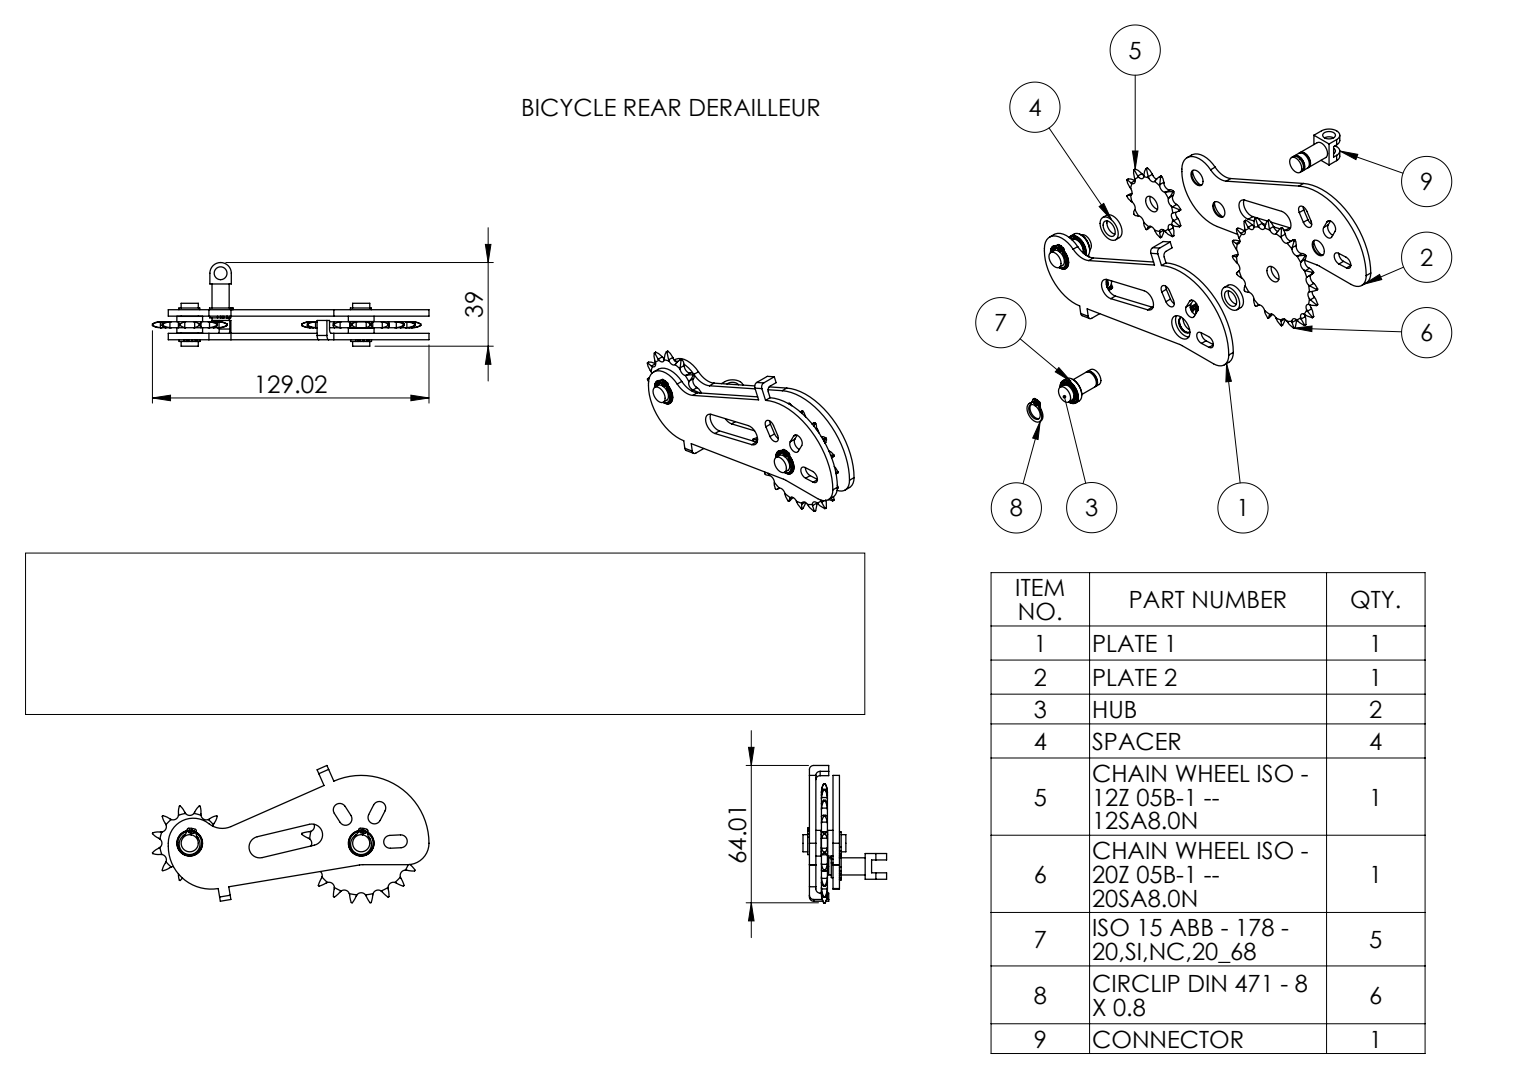
ISO-10303-21;
HEADER;
FILE_DESCRIPTION (('STEP AP214'),
    '1' );
FILE_NAME ('MAS-167',
    '2026-10-31T03:41:51',
    ( '' ),
    ( '' ),
    'SwSTEP 2.0',
    'SolidWorks 2026',
    '' );
FILE_SCHEMA (( 'AUTOMOTIVE_DESIGN' ));
ENDSEC;

DATA;
#1 = DIRECTION ( 'NONE',  ( 0.000000000000000000, 0.000000000000000000, 1.000000000000000000 ) ) ;
#2 = CARTESIAN_POINT ( 'NONE',  ( 1.749999999999998002, 19.67366047555530528, 20.02152543075352753 ) ) ;
#3 = CARTESIAN_POINT ( 'NONE',  ( 0.000000000000000000, 0.000000000000000000, 0.000000000000000000 ) ) ;
#4 = ORIENTED_EDGE ( 'NONE', *, *, #1307, .T. ) ;
#5 = CARTESIAN_POINT ( 'NONE',  ( 67.45386469005195806, 13.93318132202354676, 7.000000000000000000 ) ) ;
#6 = EDGE_LOOP ( 'NONE', ( #14602, #6535, #10108, #15176, #740, #8650, #3309 ) ) ;
#7 = DIRECTION ( 'NONE',  ( -1.000000000000000000, -0.000000000000000000, -0.000000000000000000 ) ) ;
#8 = CARTESIAN_POINT ( 'NONE',  ( 1.749999999999999778, 0.000000000000000000, 0.000000000000000000 ) ) ;
#9 = ORIENTED_EDGE ( 'NONE', *, *, #4269, .F. ) ;
#10 = ORIENTED_EDGE ( 'NONE', *, *, #14463, .T. ) ;
#11 = EDGE_CURVE ( 'NONE', #14793, #10954, #11402, .T. ) ;
#12 = CARTESIAN_POINT ( 'NONE',  ( 0.000000000000000000, 0.000000000000000000, 5.000000000000000000 ) ) ;
#13 = ORIENTED_EDGE ( 'NONE', *, *, #14923, .F. ) ;
#14 = DIRECTION ( 'NONE',  ( -0.9873505073845697533, 0.1585527532634883052, 0.000000000000000000 ) ) ;
#15 = CARTESIAN_POINT ( 'NONE',  ( 3.510166481118872639, 1.455586230640303791, -7.000000000000007994 ) ) ;
#16 = CARTESIAN_POINT ( 'NONE',  ( 0.7592463834391185440, 12.05220173035438513, 24.80264696524887214 ) ) ;
#17 = DIRECTION ( 'NONE',  ( 1.000000000000000000, 0.000000000000000000, 0.000000000000000000 ) ) ;
#18 = ORIENTED_EDGE ( 'NONE', *, *, #2231, .T. ) ;
#19 = FACE_OUTER_BOUND ( 'NONE', #11949, .T. ) ;
#20 = CARTESIAN_POINT ( 'NONE',  ( 0.02531912748631424959, 14.46287784598617243, 2.311161484776605324 ) ) ;
#21 = ORIENTED_EDGE ( 'NONE', *, *, #15147, .T. ) ;
#22 = ORIENTED_EDGE ( 'NONE', *, *, #685, .T. ) ;
#23 = CARTESIAN_POINT ( 'NONE',  ( 2.718184745196084773, 21.92234060054363809, -12.74223776959176568 ) ) ;
#24 = CARTESIAN_POINT ( 'NONE',  ( 0.006931054464085539824, -24.42321038836781355, -2.248820353273226491 ) ) ;
#25 = LINE ( 'NONE', #3651, #6082 ) ;
#26 = CARTESIAN_POINT ( 'NONE',  ( 101.4858053992934401, 0.9022481406819604643, 7.000000000000000000 ) ) ;
#27 = DIRECTION ( 'NONE',  ( 1.000000000000000000, 0.000000000000000000, 0.000000000000000000 ) ) ;
#28 = DIRECTION ( 'NONE',  ( -1.000000000000000000, 0.000000000000000000, 0.000000000000000000 ) ) ;
#29 = EDGE_CURVE ( 'NONE', #14731, #12050, #4275, .T. ) ;
#30 = ORIENTED_EDGE ( 'NONE', *, *, #9953, .F. ) ;
#31 = FACE_BOUND ( 'NONE', #5073, .T. ) ;
#32 = CARTESIAN_POINT ( 'NONE',  ( 1.039999999999997593, 0.000000000000000000, 0.000000000000000000 ) ) ;
#33 = CARTESIAN_POINT ( 'NONE',  ( 0.02531912748606228100, 5.229914364928351489, 13.68080036884350292 ) ) ;
#34 = DIRECTION ( 'NONE',  ( -1.000000000000000000, 0.000000000000000000, -0.000000000000000000 ) ) ;
#35 = VECTOR ( 'NONE', #190, 1000.000000000000000 ) ;
#36 = ORIENTED_EDGE ( 'NONE', *, *, #1393, .T. ) ;
#37 = EDGE_CURVE ( 'NONE', #40, #2037, #3752, .T. ) ;
#38 = EDGE_LOOP ( 'NONE', ( #950, #5937 ) ) ;
#39 = CARTESIAN_POINT ( 'NONE',  ( 0.07186813532171011654, 25.22589920183360945, 2.577209017047096484 ) ) ;
#40 = VERTEX_POINT ( 'NONE', #3206 ) ;
#41 = CARTESIAN_POINT ( 'NONE',  ( 2.597943782557557313, 12.05486625177586113, -10.28947301956269733 ) ) ;
#42 = CYLINDRICAL_SURFACE ( 'NONE', #425, 5.999999999999999112 ) ;
#43 = DIRECTION ( 'NONE',  ( -0.9863939238321437486, -0.1643989873053572359, 0.000000000000000000 ) ) ;
#44 = CARTESIAN_POINT ( 'NONE',  ( 67.45386469005195806, 13.93318132202354676, 4.000000000000000000 ) ) ;
#45 = FACE_OUTER_BOUND ( 'NONE', #11478, .T. ) ;
#46 = EDGE_CURVE ( 'NONE', #11802, #6223, #12333, .T. ) ;
#47 = EDGE_CURVE ( 'NONE', #3966, #1296, #12443, .T. ) ;
#48 = DIRECTION ( 'NONE',  ( 1.000000000000000000, 0.000000000000000000, 0.000000000000000000 ) ) ;
#49 = CARTESIAN_POINT ( 'NONE',  ( -14.40394475573011945, -10.79473832354794460, -3.794707603699265519E-15 ) ) ;
#50 = ORIENTED_EDGE ( 'NONE', *, *, #12668, .F. ) ;
#51 = CARTESIAN_POINT ( 'NONE',  ( 69.97572749000833880, 15.55805301486455683, 6.000000000000000000 ) ) ;
#52 = ORIENTED_EDGE ( 'NONE', *, *, #8148, .F. ) ;
#53 = B_SPLINE_CURVE_WITH_KNOTS ( 'NONE', 3,
 ( #7309, #10834, #290, #4708, #9377, #14064, #7077, #10905 ),
 .UNSPECIFIED., .F., .F.,
 ( 4, 2, 2, 4 ),
 ( 1.984117563342701228E-07, 0.001895214258086351869, 0.002842722181251365696, 0.003790230104416379524 ),
 .UNSPECIFIED. ) ;
#54 = ORIENTED_EDGE ( 'NONE', *, *, #8757, .F. ) ;
#55 = EDGE_LOOP ( 'NONE', ( #13749, #2858, #11395, #485, #2000, #143, #1377, #4123 ) ) ;
#56 = ORIENTED_EDGE ( 'NONE', *, *, #14923, .T. ) ;
#57 = DIRECTION ( 'NONE',  ( 0.9863939238321437486, 0.1643989873053572359, -0.000000000000000000 ) ) ;
#58 = EDGE_CURVE ( 'NONE', #2051, #1778, #6057, .T. ) ;
#59 = CARTESIAN_POINT ( 'NONE',  ( 2.257825459230520693, -26.58873630738055738, 4.993157874727710777 ) ) ;
#60 = CARTESIAN_POINT ( 'NONE',  ( 0.02436607992776151574, -16.37294372382871188, 18.55949924794887096 ) ) ;
#61 = DIRECTION ( 'NONE',  ( 1.000000000000000000, -0.000000000000000000, 0.000000000000000000 ) ) ;
#62 = EDGE_CURVE ( 'NONE', #4667, #5041, #11487, .T. ) ;
#63 = CARTESIAN_POINT ( 'NONE',  ( 2.021362784118872380, 12.71987259277435101, 11.98841295390602291 ) ) ;
#64 = ORIENTED_EDGE ( 'NONE', *, *, #823, .T. ) ;
#65 = DIRECTION ( 'NONE',  ( 1.000000000000000000, 0.000000000000000000, 0.000000000000000000 ) ) ;
#66 = ADVANCED_FACE ( 'NONE', ( #13569 ), #14807, .T. ) ;
#67 = PRODUCT_DEFINITION_FORMATION_WITH_SPECIFIED_SOURCE ( 'ANY', '', #14008, .NOT_KNOWN. ) ;
#68 = B_SPLINE_CURVE_WITH_KNOTS ( 'NONE', 3,
 ( #9226, #12751, #12598, #7922 ),
 .UNSPECIFIED., .F., .F.,
 ( 4, 4 ),
 ( 0.005258214619651953650, 0.005948481662034169060 ),
 .UNSPECIFIED. ) ;
#69 = ORIENTED_EDGE ( 'NONE', *, *, #13888, .F. ) ;
#70 = DIRECTION ( 'NONE',  ( -1.000000000000000000, 0.000000000000000000, -0.000000000000000000 ) ) ;
#71 = CARTESIAN_POINT ( 'NONE',  ( 2.321707774797442170, -4.824281976789052351, -0.8000000000000000444 ) ) ;
#72 = ORIENTED_EDGE ( 'NONE', *, *, #10132, .F. ) ;
#73 = ORIENTED_EDGE ( 'NONE', *, *, #10146, .F. ) ;
#74 = VECTOR ( 'NONE', #9395, 1000.000000000000000 ) ;
#75 = CARTESIAN_POINT ( 'NONE',  ( 1.039999999999996705, -20.02152543075359503, 19.67366047555523423 ) ) ;
#76 = ORIENTED_EDGE ( 'NONE', *, *, #9574, .F. ) ;
#77 = CARTESIAN_POINT ( 'NONE',  ( 1.394999999999998685, -17.29145405592685592, -4.835383649608655077 ) ) ;
#78 = DIRECTION ( 'NONE',  ( 0.000000000000000000, 0.000000000000000000, 1.000000000000000000 ) ) ;
#79 = CIRCLE ( 'NONE', #12614, 2.524999999999995914 ) ;
#80 = EDGE_CURVE ( 'NONE', #14477, #12497, #893, .T. ) ;
#81 = LINE ( 'NONE', #4807, #9670 ) ;
#82 = DIRECTION ( 'NONE',  ( 1.000000000000000000, 0.000000000000000000, 0.000000000000000000 ) ) ;
#83 = AXIS2_PLACEMENT_3D ( 'NONE', #12393, #1953, #3185 ) ;
#84 = TOROIDAL_SURFACE ( 'NONE', #8934, 5.000000000000000000, 0.5999999999999999778 ) ;
#85 = VERTEX_POINT ( 'NONE', #12565 ) ;
#86 = DIRECTION ( 'NONE',  ( -1.000000000000000000, -0.000000000000000000, 0.000000000000000000 ) ) ;
#87 = DIRECTION ( 'NONE',  ( -1.000000000000000000, 0.000000000000000000, -0.000000000000000000 ) ) ;
#88 = ORIENTED_EDGE ( 'NONE', *, *, #2042, .F. ) ;
#89 = ORIENTED_EDGE ( 'NONE', *, *, #1488, .F. ) ;
#90 = CARTESIAN_POINT ( 'NONE',  ( 0.07473575470096445461, -11.74839219818081482, -9.749517823374134196 ) ) ;
#92 = CARTESIAN_POINT ( 'NONE',  ( 0.000000000000000000, 24.34211360614310848, -7.909232158574561744 ) ) ;
#91 = AXIS2_PLACEMENT_3D ( 'NONE', #9821, #7739, #5069 ) ;
#93 = AXIS2_PLACEMENT_3D ( 'NONE', #1649, #1959, #6645 ) ;
#94 = LINE ( 'NONE', #4592, #6321 ) ;
#95 = CARTESIAN_POINT ( 'NONE',  ( -14.40394475573011945, -2.082238426203170629E-15, 16.99999999999999645 ) ) ;
#96 = DIRECTION ( 'NONE',  ( -1.000000000000000000, 0.000000000000000000, 0.000000000000000000 ) ) ;
#97 = ADVANCED_FACE ( 'NONE', ( #2039 ), #6726, .F. ) ;
#98 = DIRECTION ( 'NONE',  ( 0.000000000000000000, 0.000000000000000000, -1.000000000000000000 ) ) ;
#99 = VERTEX_POINT ( 'NONE', #962 ) ;
#100 = CARTESIAN_POINT ( 'NONE',  ( 72.68384697807672978, 11.35494834827056110, 7.000000000000000000 ) ) ;
#101 = DIRECTION ( 'NONE',  ( 0.000000000000000000, 0.000000000000000000, 1.000000000000000000 ) ) ;
#102 = DIRECTION ( 'NONE',  ( 0.9021244663126475327, 0.4314758942051350465, -1.141265444721583757E-16 ) ) ;
#103 = LINE ( 'NONE', #14195, #2432 ) ;
#104 = AXIS2_PLACEMENT_3D ( 'NONE', #9255, #12995, #7014 ) ;
#105 = DIRECTION ( 'NONE',  ( 1.000000000000000000, 0.000000000000000000, 0.000000000000000000 ) ) ;
#106 = ORIENTED_EDGE ( 'NONE', *, *, #6088, .F. ) ;
#107 = VECTOR ( 'NONE', #15180, 1000.000000000000114 ) ;
#108 = VERTEX_POINT ( 'NONE', #10337 ) ;
#109 = EDGE_CURVE ( 'NONE', #389, #2825, #14096, .T. ) ;
#110 = ORIENTED_EDGE ( 'NONE', *, *, #7513, .T. ) ;
#111 = CARTESIAN_POINT ( 'NONE',  ( 1.749999999999999778, 17.39253030560841395, -4.458161950358560333 ) ) ;
#112 = CYLINDRICAL_SURFACE ( 'NONE', #13936, 11.66666666666667318 ) ;
#113 = EDGE_CURVE ( 'NONE', #13456, #5828, #10676, .T. ) ;
#114 = CARTESIAN_POINT ( 'NONE',  ( 0.5537796329733287726, 5.139875429511856275, 16.15122426806991385 ) ) ;
#115 = CARTESIAN_POINT ( 'NONE',  ( 2.740003299868483566, 9.490919315500294218, -11.55877992729655368 ) ) ;
#116 = CARTESIAN_POINT ( 'NONE',  ( 0.000000000000000000, 0.000000000000000000, -7.000000000000008882 ) ) ;
#117 = CARTESIAN_POINT ( 'NONE',  ( 76.00000000000000000, 4.898587196589422689E-16, 6.000000000000000000 ) ) ;
#118 = CIRCLE ( 'NONE', #10455, 4.999999999999997335 ) ;
#119 = CIRCLE ( 'NONE', #7473, 14.01039946648074341 ) ;
#120 = ORIENTED_EDGE ( 'NONE', *, *, #11422, .T. ) ;
#121 = DIRECTION ( 'NONE',  ( 0.000000000000000000, 0.000000000000000000, 1.000000000000000000 ) ) ;
#122 = CARTESIAN_POINT ( 'NONE',  ( 50.00050000000000239, 0.000000000000000000, 4.000000000000000000 ) ) ;
#123 = EDGE_LOOP ( 'NONE', ( #11142, #6694, #3229, #3331, #1477 ) ) ;
#124 = DIRECTION ( 'NONE',  ( -1.000000000000000000, -0.000000000000000000, -0.000000000000000000 ) ) ;
#125 = PLANE ( 'NONE',  #1631 ) ;
#126 = PRODUCT_DEFINITION_SHAPE ( 'NONE', 'NONE',  #15227 ) ;
#127 = FILL_AREA_STYLE_COLOUR ( '', #7232 ) ;
#128 = EDGE_LOOP ( 'NONE', ( #4298, #9010, #776, #2710 ) ) ;
#129 = CIRCLE ( 'NONE', #8981, 24.12539914357697768 ) ;
#130 = EDGE_CURVE ( 'NONE', #2515, #5688, #11223, .T. ) ;
#131 = PRESENTATION_STYLE_ASSIGNMENT (( #7148 ) ) ;
#132 = VERTEX_POINT ( 'NONE', #20 ) ;
#133 = EDGE_LOOP ( 'NONE', ( #203, #10433, #5275, #14056, #9292, #1957 ) ) ;
#134 = VERTEX_POINT ( 'NONE', #3643 ) ;
#135 = CARTESIAN_POINT ( 'NONE',  ( 80.00000000000000000, 0.000000000000000000, 5.500000000000000000 ) ) ;
#136 = FACE_BOUND ( 'NONE', #13544, .T. ) ;
#137 = CARTESIAN_POINT ( 'NONE',  ( 101.6227766016837819, 5.204170427930421283E-15, -130.1575142076926852 ) ) ;
#138 = DIRECTION ( 'NONE',  ( -0.000000000000000000, -0.000000000000000000, 1.000000000000000000 ) ) ;
#139 = CIRCLE ( 'NONE', #11189, 3.799999999999999378 ) ;
#140 = EDGE_CURVE ( 'NONE', #12264, #4663, #14022, .T. ) ;
#141 = CARTESIAN_POINT ( 'NONE',  ( 0.7589665349472735079, 4.828387785248019703, 27.14933624560909919 ) ) ;
#142 = AXIS2_PLACEMENT_3D ( 'NONE', #6608, #14906, #1917 ) ;
#143 = ORIENTED_EDGE ( 'NONE', *, *, #12762, .T. ) ;
#144 = CARTESIAN_POINT ( 'NONE',  ( 0.000000000000000000, 0.000000000000000000, 3.895000000000000462 ) ) ;
#145 = VECTOR ( 'NONE', #5198, 1000.000000000000000 ) ;
#146 = EDGE_CURVE ( 'NONE', #14971, #5007, #13767, .T. ) ;
#147 = ADVANCED_FACE ( 'NONE', ( #4891 ), #11848, .T. ) ;
#148 = CIRCLE ( 'NONE', #8022, 2.524999999999995914 ) ;
#149 =( REPRESENTATION_RELATIONSHIP ('NONE','NONE', #12685, #2588 ) REPRESENTATION_RELATIONSHIP_WITH_TRANSFORMATION ( #14747 )SHAPE_REPRESENTATION_RELATIONSHIP( ) );
#150 = EDGE_LOOP ( 'NONE', ( #5698, #6923, #12784, #4888 ) ) ;
#151 = DIRECTION ( 'NONE',  ( -0.8406209333187997235, -0.5416238976136763528, 0.000000000000000000 ) ) ;
#152 = CARTESIAN_POINT ( 'NONE',  ( 1.039999999999996261, -17.29145405592685592, -4.835383649608655077 ) ) ;
#153 = EDGE_LOOP ( 'NONE', ( #4267, #3860, #12401, #12111, #6299, #3424, #1299, #11169 ) ) ;
#154 = VERTEX_POINT ( 'NONE', #3488 ) ;
#155 = AXIS2_PLACEMENT_3D ( 'NONE', #13835, #4322, #4404 ) ;
#156 = CIRCLE ( 'NONE', #8761, 0.7500000000000002220 ) ;
#157 = VECTOR ( 'NONE', #9903, 1000.000000000000000 ) ;
#158 = DIRECTION ( 'NONE',  ( 1.000000000000000000, 0.000000000000000000, 0.000000000000000000 ) ) ;
#159 = VERTEX_POINT ( 'NONE', #10494 ) ;
#160 = VECTOR ( 'NONE', #9182, 1000.000000000000000 ) ;
#161 = LINE ( 'NONE', #4805, #11382 ) ;
#162 = CARTESIAN_POINT ( 'NONE',  ( -16.14082873121598993, -7.414910804916202913, -3.000000000000000000 ) ) ;
#163 = EDGE_CURVE ( 'NONE', #12063, #1974, #3422, .T. ) ;
#164 = ADVANCED_FACE ( 'NONE', ( #8330 ), #7536, .T. ) ;
#165 = DIRECTION ( 'NONE',  ( 0.000000000000000000, 0.8660254037844327124, 0.5000000000000104361 ) ) ;
#166 = FACE_OUTER_BOUND ( 'NONE', #10902, .T. ) ;
#167 = AXIS2_PLACEMENT_3D ( 'NONE', #499, #13191, #7439 ) ;
#168 = EDGE_LOOP ( 'NONE', ( #13851, #5539, #1139, #30 ) ) ;
#169 = DIRECTION ( 'NONE',  ( -0.9148936170212769170, -0.4036950204470262649, 0.000000000000000000 ) ) ;
#170 = EDGE_CURVE ( 'NONE', #1510, #11203, #8177, .T. ) ;
#171 = CARTESIAN_POINT ( 'NONE',  ( 1.039999999999997371, 4.458161950358744186, -17.39253030560836777 ) ) ;
#172 = AXIS2_PLACEMENT_3D ( 'NONE', #5466, #3375, #833 ) ;
#173 = CIRCLE ( 'NONE', #4631, 14.01039946648074341 ) ;
#174 = ORIENTED_EDGE ( 'NONE', *, *, #12406, .F. ) ;
#175 = DIRECTION ( 'NONE',  ( 1.000000000000000000, 0.000000000000000000, 0.000000000000000000 ) ) ;
#176 = EDGE_LOOP ( 'NONE', ( #1544, #7262 ) ) ;
#177 = ORIENTED_EDGE ( 'NONE', *, *, #10181, .F. ) ;
#178 = DIRECTION ( 'NONE',  ( 0.9148936170212770280, 0.4036950204470263204, -0.000000000000000000 ) ) ;
#179 = DIRECTION ( 'NONE',  ( -0.9728364810787193395, -0.2314933715733012709, -0.000000000000000000 ) ) ;
#180 = EDGE_CURVE ( 'NONE', #10751, #7956, #7783, .T. ) ;
#181 = AXIS2_PLACEMENT_3D ( 'NONE', #7000, #4114, #12760 ) ;
#182 = CARTESIAN_POINT ( 'NONE',  ( 2.782672467460656218, 14.24942254254689189, 2.217238903388611071 ) ) ;
#183 = CARTESIAN_POINT ( 'NONE',  ( -10.00000000000000000, 0.000000000000000000, 0.000000000000000000 ) ) ;
#184 = DIRECTION ( 'NONE',  ( -1.000000000000000000, -0.000000000000000000, -0.000000000000000000 ) ) ;
#185 = AXIS2_PLACEMENT_3D ( 'NONE', #6437, #12199, #1683 ) ;
#186 = PLANE ( 'NONE',  #13689 ) ;
#187 = AXIS2_PLACEMENT_3D ( 'NONE', #8087, #3532, #12761 ) ;
#188 = VERTEX_POINT ( 'NONE', #5888 ) ;
#189 = DIRECTION ( 'NONE',  ( -1.576560579138138762E-17, 1.359337748750801608E-17, -1.000000000000000000 ) ) ;
#190 = DIRECTION ( 'NONE',  ( 1.000000000000000000, -0.000000000000000000, -0.000000000000000000 ) ) ;
#191 = DIRECTION ( 'NONE',  ( -1.000000000000000000, 0.000000000000000000, 0.000000000000000000 ) ) ;
#192 = CARTESIAN_POINT ( 'NONE',  ( 2.789999999999999147, 22.25075486061738772, 9.324097380959527115 ) ) ;
#193 = ORIENTED_EDGE ( 'NONE', *, *, #9161, .T. ) ;
#194 = ORIENTED_EDGE ( 'NONE', *, *, #4990, .T. ) ;
#195 = ORIENTED_EDGE ( 'NONE', *, *, #10486, .F. ) ;
#196 = AXIS2_PLACEMENT_3D ( 'NONE', #5704, #8149, #10157 ) ;
#197 = CARTESIAN_POINT ( 'NONE',  ( 0.02436607992775674525, 9.836394144776026138, -22.71065055754441531 ) ) ;
#198 = CARTESIAN_POINT ( 'NONE',  ( 2.789999999999999147, 1.991882183130632589, -24.04302995059963877 ) ) ;
#199 = CARTESIAN_POINT ( 'NONE',  ( 0.07473581742173406040, 5.299647274067100788, 14.31752701692938778 ) ) ;
#200 = CARTESIAN_POINT ( 'NONE',  ( 2.246812931352481613, 11.42270873787310315, -12.54666350726111901 ) ) ;
#201 = DIRECTION ( 'NONE',  ( 1.000000000000000000, 0.000000000000000000, 0.000000000000000000 ) ) ;
#202 = DIRECTION ( 'NONE',  ( -0.000000000000000000, -0.000000000000000000, -1.000000000000000000 ) ) ;
#203 = ORIENTED_EDGE ( 'NONE', *, *, #12220, .F. ) ;
#204 = FACE_OUTER_BOUND ( 'NONE', #6, .T. ) ;
#205 = DIRECTION ( 'NONE',  ( 0.000000000000000000, 0.000000000000000000, 1.000000000000000000 ) ) ;
#206 = ORIENTED_EDGE ( 'NONE', *, *, #5456, .T. ) ;
#207 = DIRECTION ( 'NONE',  ( -1.000000000000000000, -0.000000000000000000, 0.000000000000000000 ) ) ;
#208 = CARTESIAN_POINT ( 'NONE',  ( 0.07473575470096512074, 9.749517823374169723, -11.74839219818077929 ) ) ;
#209 = VECTOR ( 'NONE', #6552, 1000.000000000000114 ) ;
#210 = FACE_OUTER_BOUND ( 'NONE', #11250, .T. ) ;
#211 = EDGE_CURVE ( 'NONE', #12769, #12700, #14657, .T. ) ;
#212 = VERTEX_POINT ( 'NONE', #10569 ) ;
#213 = ORIENTED_EDGE ( 'NONE', *, *, #12762, .F. ) ;
#214 = VERTEX_POINT ( 'NONE', #2422 ) ;
#215 = ORIENTED_EDGE ( 'NONE', *, *, #3281, .T. ) ;
#216 = CARTESIAN_POINT ( 'NONE',  ( 80.00000000000000000, 0.000000000000000000, -131.1575142076926852 ) ) ;
#217 = LINE ( 'NONE', #14226, #7341 ) ;
#218 = CARTESIAN_POINT ( 'NONE',  ( 2.790000000000009805, 5.211150952915548196, -13.21889893246969905 ) ) ;
#219 = DIRECTION ( 'NONE',  ( -1.000000000000000000, -0.000000000000000000, -0.000000000000000000 ) ) ;
#220 = CIRCLE ( 'NONE', #8093, 5.999999999999999112 ) ;
#221 = LINE ( 'NONE', #525, #10167 ) ;
#222 = DIRECTION ( 'NONE',  ( -1.000000000000000000, -0.000000000000000000, -0.000000000000000000 ) ) ;
#223 = ORIENTED_EDGE ( 'NONE', *, *, #14809, .T. ) ;
#224 = DIRECTION ( 'NONE',  ( -0.000000000000000000, -0.000000000000000000, -1.000000000000000000 ) ) ;
#225 = ADVANCED_FACE ( 'NONE', ( #6882 ), #11561, .F. ) ;
#226 = CIRCLE ( 'NONE', #8834, 6.000000000000005329 ) ;
#227 = EDGE_CURVE ( 'NONE', #9499, #4705, #4811, .T. ) ;
#228 = VERTEX_POINT ( 'NONE', #7180 ) ;
#229 = CYLINDRICAL_SURFACE ( 'NONE', #11421, 13.19999999999999929 ) ;
#230 = DIRECTION ( 'NONE',  ( 0.000000000000000000, 0.000000000000000000, 1.000000000000000000 ) ) ;
#231 = ORIENTED_EDGE ( 'NONE', *, *, #8908, .F. ) ;
#232 = ORIENTED_EDGE ( 'NONE', *, *, #7399, .F. ) ;
#233 = DIRECTION ( 'NONE',  ( 1.000000000000000000, 0.000000000000000000, 0.000000000000000000 ) ) ;
#234 = ADVANCED_FACE ( 'NONE', ( #9266 ), #13953, .F. ) ;
#235 = ORIENTED_EDGE ( 'NONE', *, *, #9615, .F. ) ;
#236 = ADVANCED_FACE ( 'NONE', ( #12247, #14409 ), #3875, .F. ) ;
#237 = CARTESIAN_POINT ( 'NONE',  ( -1.250000000000001110, 7.286648454926751965E-16, 5.899999999999999467 ) ) ;
#238 = CARTESIAN_POINT ( 'NONE',  ( 2.740003288479521348, -14.75565684666125144, -2.439987328297124947 ) ) ;
#239 = DIRECTION ( 'NONE',  ( 0.9728364810787194505, 0.2314933715733012709, -0.000000000000000000 ) ) ;
#240 = CARTESIAN_POINT ( 'NONE',  ( 0.000000000000000000, 0.000000000000000000, 4.500000000000000888 ) ) ;
#241 = VERTEX_POINT ( 'NONE', #12080 ) ;
#242 = B_SPLINE_CURVE_WITH_KNOTS ( 'NONE', 3,
 ( #7619, #12222, #12296, #11068, #11983, #9993, #527, #1623 ),
 .UNSPECIFIED., .F., .F.,
 ( 4, 2, 2, 4 ),
 ( 2.445728210258510103E-07, 0.001895260649874687441, 0.002842768688401517505, 0.003790276726928347353 ),
 .UNSPECIFIED. ) ;
#243 = CARTESIAN_POINT ( 'NONE',  ( 31.51081190520435626, 3.030430839836910639, 2.999999999999999112 ) ) ;
#244 = LINE ( 'NONE', #4960, #10717 ) ;
#245 = EDGE_LOOP ( 'NONE', ( #3924, #9701, #3037, #7641 ) ) ;
#246 = CARTESIAN_POINT ( 'NONE',  ( 10.40394475573011945, -10.79473832354794460, 6.000000000000000000 ) ) ;
#247 = ORIENTED_EDGE ( 'NONE', *, *, #4486, .T. ) ;
#248 = ORIENTED_EDGE ( 'NONE', *, *, #1307, .F. ) ;
#249 = EDGE_CURVE ( 'NONE', #5007, #12521, #11742, .T. ) ;
#250 = CARTESIAN_POINT ( 'NONE',  ( -5.999999999999999112, 0.000000000000000000, 3.000000000000000000 ) ) ;
#251 = DIRECTION ( 'NONE',  ( -1.000000000000000000, 0.000000000000000000, -0.000000000000000000 ) ) ;
#252 = ADVANCED_FACE ( 'NONE', ( #6406, #6332 ), #7416, .F. ) ;
#253 =( LENGTH_UNIT ( ) NAMED_UNIT ( * ) SI_UNIT ( .MILLI., .METRE. ) );
#254 = CARTESIAN_POINT ( 'NONE',  ( 0.07181525696555157712, 5.344212458769712626, -24.78695292654915860 ) ) ;
#255 = LINE ( 'NONE', #4972, #14719 ) ;
#256 = PRODUCT_DEFINITION_SHAPE ( 'NONE', 'NONE',  #13870 ) ;
#257 = EDGE_CURVE ( 'NONE', #8622, #3271, #11448, .T. ) ;
#258 = CARTESIAN_POINT ( 'NONE',  ( 0.02531912748464848137, 2.311161484776556030, 14.46287784598618309 ) ) ;
#259 = EDGE_LOOP ( 'NONE', ( #3282, #14256 ) ) ;
#260 = DIRECTION ( 'NONE',  ( 0.000000000000000000, 0.000000000000000000, -1.000000000000000000 ) ) ;
#261 = DIRECTION ( 'NONE',  ( -2.081668171172168513E-16, 1.000000000000000000, 0.000000000000000000 ) ) ;
#262 = CARTESIAN_POINT ( 'NONE',  ( 2.337784062669523877, -3.429166897524313029, -16.32199768300083420 ) ) ;
#263 = DIRECTION ( 'NONE',  ( 0.000000000000000000, 0.000000000000000000, -1.000000000000000000 ) ) ;
#264 = EDGE_CURVE ( 'NONE', #12037, #12700, #1561, .T. ) ;
#265 = EDGE_LOOP ( 'NONE', ( #1777, #5909, #7218, #13127 ) ) ;
#266 = EDGE_LOOP ( 'NONE', ( #5592, #13272, #13522, #7221 ) ) ;
#267 = VECTOR ( 'NONE', #3874, 1000.000000000000000 ) ;
#268 = B_SPLINE_CURVE_WITH_KNOTS ( 'NONE', 3,
 ( #6737, #12274, #4444, #11193 ),
 .UNSPECIFIED., .F., .F.,
 ( 4, 4 ),
 ( 0.005258120783916825358, 0.005948386350302978416 ),
 .UNSPECIFIED. ) ;
#269 = VERTEX_POINT ( 'NONE', #10859 ) ;
#270 = CARTESIAN_POINT ( 'NONE',  ( 2.789999999999999147, -24.04302995059964587, -1.991882183130548878 ) ) ;
#271 = DIRECTION ( 'NONE',  ( -0.000000000000000000, -0.000000000000000000, -1.000000000000000000 ) ) ;
#272 = DIRECTION ( 'NONE',  ( 0.02857142857142857401, -0.9995917534020515305, 0.000000000000000000 ) ) ;
#273 = CARTESIAN_POINT ( 'NONE',  ( 1.749999999999998002, -27.68468304288262516, 4.633866840648810381 ) ) ;
#274 = DIRECTION ( 'NONE',  ( 0.000000000000000000, 0.000000000000000000, -1.000000000000000000 ) ) ;
#275 = LINE ( 'NONE', #354, #6695 ) ;
#276 = ORIENTED_EDGE ( 'NONE', *, *, #3938, .F. ) ;
#277 = CYLINDRICAL_SURFACE ( 'NONE', #11037, 13.19999999999999574 ) ;
#278 = CYLINDRICAL_SURFACE ( 'NONE', #5273, 4.000000000000003553 ) ;
#279 = ORIENTED_EDGE ( 'NONE', *, *, #14874, .F. ) ;
#280 = CARTESIAN_POINT ( 'NONE',  ( 0.000000000000000000, 0.000000000000000000, -0.8000000000000000444 ) ) ;
#281 = AXIS2_PLACEMENT_3D ( 'NONE', #6195, #5139, #2580 ) ;
#282 = DIRECTION ( 'NONE',  ( 0.000000000000000000, 0.000000000000000000, 1.000000000000000000 ) ) ;
#283 = CARTESIAN_POINT ( 'NONE',  ( 2.789999999999999147, 3.120158876139233595, -14.59528211759998939 ) ) ;
#284 = ORIENTED_EDGE ( 'NONE', *, *, #11327, .F. ) ;
#285 = CARTESIAN_POINT ( 'NONE',  ( 0.1085714285714285687, -3.798448662927795372, 0.000000000000000000 ) ) ;
#286 = ORIENTED_EDGE ( 'NONE', *, *, #13802, .T. ) ;
#287 = EDGE_LOOP ( 'NONE', ( #9306, #900, #54, #10982, #12376 ) ) ;
#288 = ORIENTED_EDGE ( 'NONE', *, *, #5024, .T. ) ;
#289 = DIRECTION ( 'NONE',  ( 1.000000000000000000, 0.000000000000000000, -0.000000000000000000 ) ) ;
#290 = CARTESIAN_POINT ( 'NONE',  ( 0.1920564340659368652, -5.295083827234610574, -14.93837896275555721 ) ) ;
#291 = VECTOR ( 'NONE', #10020, 999.9999999999998863 ) ;
#292 = VECTOR ( 'NONE', #261, 1000.000000000000000 ) ;
#293 = CARTESIAN_POINT ( 'NONE',  ( 2.782650494170371580, 5.204557061642474558, -13.44926448535260377 ) ) ;
#294 = DIRECTION ( 'NONE',  ( -1.000000000000000000, -0.000000000000000000, -0.000000000000000000 ) ) ;
#295 = CARTESIAN_POINT ( 'NONE',  ( 0.000000000000000000, -8.936381166381891568E-14, 25.59481291497571220 ) ) ;
#296 = LINE ( 'NONE', #6688, #7102 ) ;
#297 = EDGE_CURVE ( 'NONE', #1055, #15218, #8747, .T. ) ;
#298 = ORIENTED_EDGE ( 'NONE', *, *, #4470, .F. ) ;
#299 = B_SPLINE_CURVE_WITH_KNOTS ( 'NONE', 3,
 ( #2873, #12317, #14722, #1958 ),
 .UNSPECIFIED., .F., .F.,
 ( 4, 4 ),
 ( 0.005540500595652399218, 0.005814376014856854034 ),
 .UNSPECIFIED. ) ;
#300 = LINE ( 'NONE', #8227, #4591 ) ;
#301 = CIRCLE ( 'NONE', #10863, 28.06981291497571362 ) ;
#302 = ORIENTED_EDGE ( 'NONE', *, *, #9017, .F. ) ;
#303 = ORIENTED_EDGE ( 'NONE', *, *, #14839, .T. ) ;
#304 = B_SPLINE_CURVE_WITH_KNOTS ( 'NONE', 3,
 ( #13132, #218, #293, #11828 ),
 .UNSPECIFIED., .F., .F.,
 ( 4, 4 ),
 ( 0.005123742438166219160, 0.005814376014856852300 ),
 .UNSPECIFIED. ) ;
#305 = CYLINDRICAL_SURFACE ( 'NONE', #14089, 28.06981291497571362 ) ;
#306 = ADVANCED_FACE ( 'NONE', ( #9862 ), #2790, .F. ) ;
#307 = LINE ( 'NONE', #10624, #1105 ) ;
#308 = ORIENTED_EDGE ( 'NONE', *, *, #8675, .F. ) ;
#309 = EDGE_CURVE ( 'NONE', #2455, #13045, #11550, .T. ) ;
#310 = FACE_OUTER_BOUND ( 'NONE', #10572, .T. ) ;
#311 = ORIENTED_EDGE ( 'NONE', *, *, #14820, .T. ) ;
#312 = DIRECTION ( 'NONE',  ( 0.000000000000000000, 0.000000000000000000, 1.000000000000000000 ) ) ;
#313 = EDGE_CURVE ( 'NONE', #13918, #6218, #8504, .T. ) ;
#314 = DIRECTION ( 'NONE',  ( -0.000000000000000000, -0.000000000000000000, -1.000000000000000000 ) ) ;
#315 = CARTESIAN_POINT ( 'NONE',  ( 2.789999999999999147, 15.74360496233381390, 18.28042085475283685 ) ) ;
#316 = VERTEX_POINT ( 'NONE', #2870 ) ;
#317 = CARTESIAN_POINT ( 'NONE',  ( 0.5279273381794611364, 3.461047254864636713, -26.82026385750174668 ) ) ;
#318 = CARTESIAN_POINT ( 'NONE',  ( 2.789999999999999147, 20.70663861606272249, 15.04425356660767932 ) ) ;
#319 = ORIENTED_EDGE ( 'NONE', *, *, #11799, .F. ) ;
#320 = DIRECTION ( 'NONE',  ( 0.000000000000000000, 0.000000000000000000, 1.000000000000000000 ) ) ;
#321 = EDGE_CURVE ( 'NONE', #3392, #9499, #13955, .T. ) ;
#322 = CARTESIAN_POINT ( 'NONE',  ( 0.1855656748306453718, 25.77772010606605946, 2.851997810081739360 ) ) ;
#323 = ORIENTED_EDGE ( 'NONE', *, *, #9187, .T. ) ;
#324 = EDGE_LOOP ( 'NONE', ( #378, #14042, #4793, #7094 ) ) ;
#325 = DIRECTION ( 'NONE',  ( -1.000000000000000000, -0.000000000000000000, -0.000000000000000000 ) ) ;
#326 = DIRECTION ( 'NONE',  ( 0.000000000000000000, 0.000000000000000000, 1.000000000000000000 ) ) ;
#327 = B_SPLINE_CURVE_WITH_KNOTS ( 'NONE', 3,
 ( #9952, #1804, #5582, #14799 ),
 .UNSPECIFIED., .F., .F.,
 ( 4, 4 ),
 ( 0.005123713096549426665, 0.005814346476695865691 ),
 .UNSPECIFIED. ) ;
#328 = SURFACE_STYLE_USAGE ( .BOTH. , #10800 ) ;
#329 = FACE_OUTER_BOUND ( 'NONE', #10914, .T. ) ;
#330 = CIRCLE ( 'NONE', #3305, 2.999999999999988898 ) ;
#331 = EDGE_CURVE ( 'NONE', #13647, #13720, #7540, .T. ) ;
#332 = DIRECTION ( 'NONE',  ( 1.000000000000000000, 0.000000000000000000, 0.000000000000000000 ) ) ;
#333 = TOROIDAL_SURFACE ( 'NONE', #14843, 24.12539914357697768, 8.000000000000000000 ) ;
#334 = EDGE_LOOP ( 'NONE', ( #5406, #2632 ) ) ;
#335 = DIRECTION ( 'NONE',  ( 1.000000000000000000, 0.000000000000000000, 0.000000000000000000 ) ) ;
#336 = AXIS2_PLACEMENT_3D ( 'NONE', #12347, #8023, #13657 ) ;
#337 = DIRECTION ( 'NONE',  ( 1.000000000000000000, 0.000000000000000000, 0.000000000000000000 ) ) ;
#338 = CARTESIAN_POINT ( 'NONE',  ( 0.0003207540509381473352, -20.70663861606275447, -12.51925356660783528 ) ) ;
#339 = CARTESIAN_POINT ( 'NONE',  ( 2.790000000000000480, -18.34424029220122776, 15.96500990068118497 ) ) ;
#340 = EDGE_CURVE ( 'NONE', #7818, #11509, #2563, .T. ) ;
#341 = ORIENTED_EDGE ( 'NONE', *, *, #8187, .F. ) ;
#342 = ORIENTED_EDGE ( 'NONE', *, *, #10454, .F. ) ;
#343 = CIRCLE ( 'NONE', #11635, 2.524999999999998579 ) ;
#344 = EDGE_CURVE ( 'NONE', #1013, #13731, #244, .T. ) ;
#345 = ADVANCED_FACE ( 'NONE', ( #14325 ), #11163, .T. ) ;
#346 = AXIS2_PLACEMENT_3D ( 'NONE', #7761, #8835, #8986 ) ;
#347 = ORIENTED_EDGE ( 'NONE', *, *, #9380, .F. ) ;
#348 = VECTOR ( 'NONE', #6757, 1000.000000000000000 ) ;
#349 = CYLINDRICAL_SURFACE ( 'NONE', #13438, 4.000000000000000000 ) ;
#350 = CARTESIAN_POINT ( 'NONE',  ( 5.139549990269394683E-16, -2.133490293297187979, 24.22479935914660132 ) ) ;
#351 = DIRECTION ( 'NONE',  ( -0.000000000000000000, -0.000000000000000000, -1.000000000000000000 ) ) ;
#352 = DIRECTION ( 'NONE',  ( -1.000000000000000000, 0.000000000000000000, 0.000000000000000000 ) ) ;
#353 = DIRECTION ( 'NONE',  ( -0.9873505073845697533, 0.1585527532634883052, -5.103307673902844724E-17 ) ) ;
#354 = CARTESIAN_POINT ( 'NONE',  ( -1.000000000000000222, -4.808326913195983821, 0.000000000000000000 ) ) ;
#355 = ORIENTED_EDGE ( 'NONE', *, *, #8570, .F. ) ;
#356 = DIRECTION ( 'NONE',  ( 0.000000000000000000, -0.000000000000000000, -1.000000000000000000 ) ) ;
#357 = FACE_OUTER_BOUND ( 'NONE', #5702, .T. ) ;
#358 = ORIENTED_EDGE ( 'NONE', *, *, #7383, .F. ) ;
#359 = DIRECTION ( 'NONE',  ( 1.000000000000000000, 0.000000000000000000, 0.000000000000000000 ) ) ;
#360 = DIRECTION ( 'NONE',  ( -0.000000000000000000, -0.000000000000000000, -1.000000000000000000 ) ) ;
#361 = AXIS2_PLACEMENT_3D ( 'NONE', #2405, #5025, #1550 ) ;
#362 = CARTESIAN_POINT ( 'NONE',  ( 0.000000000000000000, -5.249430348645841349, 12.98979500319692626 ) ) ;
#363 = ORIENTED_EDGE ( 'NONE', *, *, #14313, .F. ) ;
#364 = EDGE_CURVE ( 'NONE', #6867, #6366, #11210, .T. ) ;
#365 = CARTESIAN_POINT ( 'NONE',  ( 0.04999670013151490816, -11.55877992729671888, 9.490919315500097042 ) ) ;
#366 = CARTESIAN_POINT ( 'NONE',  ( 0.02436607992776541887, 12.59161484032942901, -21.30679549418617924 ) ) ;
#367 = VERTEX_POINT ( 'NONE', #13477 ) ;
#368 = VERTEX_POINT ( 'NONE', #2951 ) ;
#369 = ORIENTED_EDGE ( 'NONE', *, *, #4930, .F. ) ;
#370 = DIRECTION ( 'NONE',  ( -0.000000000000000000, -0.000000000000000000, -1.000000000000000000 ) ) ;
#371 = CIRCLE ( 'NONE', #5552, 0.5999999999999998668 ) ;
#372 = DIRECTION ( 'NONE',  ( -0.000000000000000000, -0.000000000000000000, 1.000000000000000000 ) ) ;
#373 = CARTESIAN_POINT ( 'NONE',  ( 0.07473579423048590242, -15.04916547791952119, -2.569134216959054751 ) ) ;
#374 = CARTESIAN_POINT ( 'NONE',  ( 2.764680872513207266, -9.232963481057685939, -11.36963888406697087 ) ) ;
#375 = DIRECTION ( 'NONE',  ( 0.000000000000000000, 0.000000000000000000, 1.000000000000000000 ) ) ;
#376 = EDGE_CURVE ( 'NONE', #14085, #567, #7640, .T. ) ;
#377 = CARTESIAN_POINT ( 'NONE',  ( -14.40394475573011768, -13.79473832354794993, 16.99999999999999645 ) ) ;
#378 = ORIENTED_EDGE ( 'NONE', *, *, #2401, .F. ) ;
#379 = CARTESIAN_POINT ( 'NONE',  ( -7.595268335593441642E-14, -22.38018801136484015, 9.515416771311118183 ) ) ;
#380 = VECTOR ( 'NONE', #3922, 1000.000000000000000 ) ;
#381 = SURFACE_SIDE_STYLE ('',( #533 ) ) ;
#382 = ORIENTED_EDGE ( 'NONE', *, *, #13166, .T. ) ;
#383 = VERTEX_POINT ( 'NONE', #7122 ) ;
#384 = DIRECTION ( 'NONE',  ( 0.000000000000000000, 0.000000000000000000, 1.000000000000000000 ) ) ;
#385 = CARTESIAN_POINT ( 'NONE',  ( -16.02604379927987566, -7.138402084508245871, -3.000000000000000444 ) ) ;
#386 = EDGE_CURVE ( 'NONE', #14639, #7731, #1893, .T. ) ;
#387 = AXIS2_PLACEMENT_3D ( 'NONE', #8515, #438, #8738 ) ;
#388 = B_SPLINE_CURVE_WITH_KNOTS ( 'NONE', 3,
 ( #10440, #12588, #1999, #9069 ),
 .UNSPECIFIED., .F., .F.,
 ( 4, 4 ),
 ( 1.988537749986050620E-07, 0.0006916721208754040336 ),
 .UNSPECIFIED. ) ;
#389 = VERTEX_POINT ( 'NONE', #11725 ) ;
#390 = CIRCLE ( 'NONE', #4832, 2.524999999999996358 ) ;
#391 = UNCERTAINTY_MEASURE_WITH_UNIT (LENGTH_MEASURE( 1.000000000000000082E-05 ), #9778, 'distance_accuracy_value', 'NONE');
#392 = LINE ( 'NONE', #9787, #6528 ) ;
#393 = VERTEX_POINT ( 'NONE', #7047 ) ;
#394 = CARTESIAN_POINT ( 'NONE',  ( 0.000000000000000000, -15.04425356660744839, -18.18163861606288378 ) ) ;
#395 = CARTESIAN_POINT ( 'NONE',  ( 0.000000000000000000, -5.249430348645841349, 12.98979500319692626 ) ) ;
#396 = CARTESIAN_POINT ( 'NONE',  ( 0.000000000000000000, 7.909232158575156824, -21.81711360614291806 ) ) ;
#397 = TOROIDAL_SURFACE ( 'NONE', #10724, 14.01039946648073986, 8.000000000000000000 ) ;
#398 = CARTESIAN_POINT ( 'NONE',  ( 1.039999999999995595, 4.147968289691676524, -27.76164181293047051 ) ) ;
#399 = EDGE_CURVE ( 'NONE', #5499, #5314, #14702, .T. ) ;
#400 = CARTESIAN_POINT ( 'NONE',  ( 0.7589665326895891351, 12.98167595241022276, 24.32849926382755257 ) ) ;
#401 = AXIS2_PLACEMENT_3D ( 'NONE', #216, #3759, #10608 ) ;
#402 = ORIENTED_EDGE ( 'NONE', *, *, #5553, .T. ) ;
#403 = AXIS2_PLACEMENT_3D ( 'NONE', #7843, #9071, #11364 ) ;
#404 = CARTESIAN_POINT ( 'NONE',  ( 1.039999999999997593, -4.458161950358380032, -17.39253030560846369 ) ) ;
#405 = ORIENTED_EDGE ( 'NONE', *, *, #2597, .T. ) ;
#406 = VERTEX_POINT ( 'NONE', #13971 ) ;
#407 = DIRECTION ( 'NONE',  ( -1.000000000000000000, -0.000000000000000000, 0.000000000000000000 ) ) ;
#408 = CARTESIAN_POINT ( 'NONE',  ( 1.749999999999998002, 4.633866840648922292, 27.68468304288260384 ) ) ;
#409 = AXIS2_PLACEMENT_3D ( 'NONE', #13820, #7911, #6613 ) ;
#410 = CARTESIAN_POINT ( 'NONE',  ( 2.789999999999999147, -14.55412442567604003, -19.64056340710890325 ) ) ;
#411 = ORIENTED_EDGE ( 'NONE', *, *, #420, .T. ) ;
#412 = LINE ( 'NONE', #6346, #4643 ) ;
#413 = DIRECTION ( 'NONE',  ( -0.000000000000000000, -0.000000000000000000, 1.000000000000000000 ) ) ;
#414 = VECTOR ( 'NONE', #3445, 1000.000000000000114 ) ;
#415 = CIRCLE ( 'NONE', #14963, 5.000000000000000888 ) ;
#416 = DIRECTION ( 'NONE',  ( 1.576560579138138762E-17, -1.359337748750801608E-17, 1.000000000000000000 ) ) ;
#417 = DIRECTION ( 'NONE',  ( 1.000000000000000000, 0.000000000000000000, -0.000000000000000000 ) ) ;
#418 = VERTEX_POINT ( 'NONE', #1273 ) ;
#419 = ORIENTED_EDGE ( 'NONE', *, *, #12361, .F. ) ;
#420 = EDGE_CURVE ( 'NONE', #2610, #7436, #6553, .T. ) ;
#421 = ORIENTED_EDGE ( 'NONE', *, *, #8347, .F. ) ;
#422 = PRESENTATION_LAYER_ASSIGNMENT (  '', '', ( #10019 ) ) ;
#423 = DIRECTION ( 'NONE',  ( 0.000000000000000000, 0.000000000000000000, 1.000000000000000000 ) ) ;
#424 = DIRECTION ( 'NONE',  ( -1.000000000000000000, 0.000000000000000000, -0.000000000000000000 ) ) ;
#425 = AXIS2_PLACEMENT_3D ( 'NONE', #3589, #8419, #2592 ) ;
#426 = CIRCLE ( 'NONE', #5853, 4.999999999999999112 ) ;
#427 = LINE ( 'NONE', #11042, #5355 ) ;
#428 = DIRECTION ( 'NONE',  ( -0.9975010064204038462, 0.07065226245691945406, 0.000000000000000000 ) ) ;
#429 = DIRECTION ( 'NONE',  ( 0.000000000000000000, 0.000000000000000000, 1.000000000000000000 ) ) ;
#430 = ORIENTED_EDGE ( 'NONE', *, *, #3464, .T. ) ;
#431 = FACE_OUTER_BOUND ( 'NONE', #11888, .T. ) ;
#432 = CARTESIAN_POINT ( 'NONE',  ( 2.262072637928881580, 12.96450951081251191, -23.73240184472483350 ) ) ;
#433 = PRODUCT_RELATED_PRODUCT_CATEGORY ( 'part', '', ( #6388 ) ) ;
#434 = EDGE_CURVE ( 'NONE', #952, #7149, #14309, .T. ) ;
#435 = ORIENTED_EDGE ( 'NONE', *, *, #10644, .T. ) ;
#436 = DIRECTION ( 'NONE',  ( 1.000000000000000000, 0.000000000000000000, 0.000000000000000000 ) ) ;
#437 = EDGE_CURVE ( 'NONE', #12266, #2494, #3436, .T. ) ;
#438 = DIRECTION ( 'NONE',  ( -0.000000000000000000, -1.000000000000000000, -0.000000000000000000 ) ) ;
#439 = VECTOR ( 'NONE', #10989, 1000.000000000000000 ) ;
#440 = CARTESIAN_POINT ( 'NONE',  ( 1.749999999999998002, -24.89775460606821866, -12.96210679857815684 ) ) ;
#441 = ORIENTED_EDGE ( 'NONE', *, *, #8796, .T. ) ;
#442 = AXIS2_PLACEMENT_3D ( 'NONE', #13011, #2427, #5893 ) ;
#443 = AXIS2_PLACEMENT_3D ( 'NONE', #14732, #958, #12498 ) ;
#444 = CARTESIAN_POINT ( 'NONE',  ( 2.508169719062756986, -10.58084377126631814, 12.18203740414262803 ) ) ;
#445 = CARTESIAN_POINT ( 'NONE',  ( 19.25177984293775424, 7.759396820770413150, 6.000000000000005329 ) ) ;
#446 = VERTEX_POINT ( 'NONE', #11865 ) ;
#447 = VERTEX_POINT ( 'NONE', #12796 ) ;
#448 = VERTEX_POINT ( 'NONE', #8125 ) ;
#449 = CARTESIAN_POINT ( 'NONE',  ( 4.000000000000000000, 4.898587196589412829E-16, 7.000000000000000000 ) ) ;
#450 = CARTESIAN_POINT ( 'NONE',  ( 0.6102186610125081012, 23.94322454545469370, 12.96989951879415770 ) ) ;
#451 = CARTESIAN_POINT ( 'NONE',  ( 2.782672435525938237, 9.044896821682357313, -11.23174270417319676 ) ) ;
#452 = CARTESIAN_POINT ( 'NONE',  ( 2.764680872515352661, -2.311161484776655950, 14.46287784598616355 ) ) ;
#453 = EDGE_CURVE ( 'NONE', #2791, #11000, #13669, .T. ) ;
#454 = DIRECTION ( 'NONE',  ( -1.000000000000000000, 0.000000000000000000, 0.000000000000000000 ) ) ;
#455 = ADVANCED_FACE ( 'NONE', ( #8054 ), #3901, .T. ) ;
#456 = CARTESIAN_POINT ( 'NONE',  ( 2.262072706628475149, 19.66369668717060293, -18.56460150496918260 ) ) ;
#457 = CIRCLE ( 'NONE', #14962, 24.12539914357697413 ) ;
#458 = CIRCLE ( 'NONE', #14217, 28.06981291497571362 ) ;
#459 = CIRCLE ( 'NONE', #717, 20.00000000000000000 ) ;
#460 = EDGE_CURVE ( 'NONE', #5313, #7859, #6354, .T. ) ;
#461 = ORIENTED_EDGE ( 'NONE', *, *, #12360, .F. ) ;
#462 = CARTESIAN_POINT ( 'NONE',  ( 0.000000000000000000, 0.000000000000000000, 0.000000000000000000 ) ) ;
#463 = ADVANCED_FACE ( 'NONE', ( #9503 ), #15129, .T. ) ;
#464 = PRESENTATION_STYLE_ASSIGNMENT (( #1775 ) ) ;
#465 = ORIENTED_EDGE ( 'NONE', *, *, #12135, .F. ) ;
#466 = ORIENTED_EDGE ( 'NONE', *, *, #12652, .F. ) ;
#467 = CIRCLE ( 'NONE', #9076, 28.06981291497571362 ) ;
#468 = CARTESIAN_POINT ( 'NONE',  ( 1.039999999999996261, -4.835383649608352208, -17.29145405592693763 ) ) ;
#469 = B_SPLINE_CURVE_WITH_KNOTS ( 'NONE', 3,
 ( #4535, #14047, #3516, #14126, #2370, #7062 ),
 .UNSPECIFIED., .F., .F.,
 ( 4, 2, 4 ),
 ( 4.462636682232942879E-07, 0.001879885020955589887, 0.003759323778242956802 ),
 .UNSPECIFIED. ) ;
#470 = ORIENTED_EDGE ( 'NONE', *, *, #13886, .T. ) ;
#471 = B_SPLINE_CURVE_WITH_KNOTS ( 'NONE', 3,
 ( #9307, #4845, #14216, #12817 ),
 .UNSPECIFIED., .F., .F.,
 ( 4, 4 ),
 ( 0.005258139959819249469, 0.005948405594583416715 ),
 .UNSPECIFIED. ) ;
#472 = CARTESIAN_POINT ( 'NONE',  ( -10.00000000000000000, 0.000000000000000000, 0.000000000000000000 ) ) ;
#473 = ORIENTED_EDGE ( 'NONE', *, *, #8532, .T. ) ;
#474 = CARTESIAN_POINT ( 'NONE',  ( 0.02436607992776628623, 24.63872515616082737, -2.336989772644355590 ) ) ;
#475 = DIRECTION ( 'NONE',  ( 1.000000000000000000, 0.000000000000000000, 0.000000000000000000 ) ) ;
#476 = ADVANCED_BREP_SHAPE_REPRESENTATION ( '', ( #9040, #1376 ), #13900 ) ;
#477 = CIRCLE ( 'NONE', #9084, 17.95481323787947403 ) ;
#478 = LINE ( 'NONE', #13313, #9423 ) ;
#479 = DIRECTION ( 'NONE',  ( -0.9995917534020515305, -0.02857142857142857054, 0.000000000000000000 ) ) ;
#480 = CARTESIAN_POINT ( 'NONE',  ( -9.999999999999998224, 0.000000000000000000, -131.1575142076926852 ) ) ;
#481 = ORIENTED_EDGE ( 'NONE', *, *, #1964, .T. ) ;
#482 = FACE_OUTER_BOUND ( 'NONE', #14654, .T. ) ;
#483 = DIRECTION ( 'NONE',  ( -1.000000000000000000, 0.000000000000000000, 0.000000000000000000 ) ) ;
#484 = VERTEX_POINT ( 'NONE', #9353 ) ;
#485 = ORIENTED_EDGE ( 'NONE', *, *, #6558, .T. ) ;
#486 = CIRCLE ( 'NONE', #11774, 14.01039946648074341 ) ;
#487 = CYLINDRICAL_SURFACE ( 'NONE', #11244, 5.999999999999999112 ) ;
#488 = CYLINDRICAL_SURFACE ( 'NONE', #10200, 2.524999999999999467 ) ;
#489 = CARTESIAN_POINT ( 'NONE',  ( 2.789999999999999147, 8.624777288397799779, 11.04103753892274753 ) ) ;
#490 = ORIENTED_EDGE ( 'NONE', *, *, #9421, .T. ) ;
#491 = CARTESIAN_POINT ( 'NONE',  ( 67.23404255319148604, 28.93147646537027384, -131.1575142076926852 ) ) ;
#492 = B_SPLINE_CURVE_WITH_KNOTS ( 'NONE', 3,
 ( #6585, #14735, #5589, #12414, #5439, #11333 ),
 .UNSPECIFIED., .F., .F.,
 ( 4, 2, 4 ),
 ( 2.321268216996885854E-07, 0.001878622960950492504, 0.003757013795079285415 ),
 .UNSPECIFIED. ) ;
#493 = FACE_OUTER_BOUND ( 'NONE', #2373, .T. ) ;
#494 = CARTESIAN_POINT ( 'NONE',  ( 2.789999999999999147, -7.909232158574647009, -24.34211360614308006 ) ) ;
#495 = VERTEX_POINT ( 'NONE', #11574 ) ;
#496 = ORIENTED_EDGE ( 'NONE', *, *, #10416, .F. ) ;
#497 = VERTEX_POINT ( 'NONE', #5831 ) ;
#498 = B_SPLINE_CURVE_WITH_KNOTS ( 'NONE', 3,
 ( #4619, #8065, #4302, #10295 ),
 .UNSPECIFIED., .F., .F.,
 ( 4, 4 ),
 ( 2.159563976372916968E-07, 0.0006916893629248549880 ),
 .UNSPECIFIED. ) ;
#499 = CARTESIAN_POINT ( 'NONE',  ( 8.000000000000000000, 0.000000000000000000, 0.000000000000000000 ) ) ;
#500 = DIRECTION ( 'NONE',  ( 0.000000000000000000, 0.000000000000000000, 1.000000000000000000 ) ) ;
#501 = DIRECTION ( 'NONE',  ( -1.000000000000000000, 0.000000000000000000, 0.000000000000000000 ) ) ;
#502 = CARTESIAN_POINT ( 'NONE',  ( 2.789999999999999147, -7.772527002114268058, -23.17675759782048672 ) ) ;
#503 = APPLICATION_PROTOCOL_DEFINITION ( 'draft international standard', 'automotive_design', 1998, #2917 ) ;
#504 = CARTESIAN_POINT ( 'NONE',  ( 1.885839510111768869, 4.928563447326528291, -17.01651022436359284 ) ) ;
#505 = EDGE_CURVE ( 'NONE', #1110, #13796, #457, .T. ) ;
#506 = CARTESIAN_POINT ( 'NONE',  ( 1.039999999999997371, 4.458161950358744186, -17.39253030560836777 ) ) ;
#507 = CARTESIAN_POINT ( 'NONE',  ( -3.799999999999999378, 4.653657836759941744E-16, -0.8000000000000000444 ) ) ;
#508 = ORIENTED_EDGE ( 'NONE', *, *, #8414, .T. ) ;
#509 = DIRECTION ( 'NONE',  ( 0.000000000000000000, 0.000000000000000000, 1.000000000000000000 ) ) ;
#510 = CARTESIAN_POINT ( 'NONE',  ( -10.00000000000000000, 0.000000000000000000, 0.000000000000000000 ) ) ;
#511 = EDGE_CURVE ( 'NONE', #12603, #7404, #14471, .T. ) ;
#512 = CARTESIAN_POINT ( 'NONE',  ( 2.179781338987520467, -23.94322454545470436, 12.96989951879399072 ) ) ;
#513 = ORIENTED_EDGE ( 'NONE', *, *, #4652, .F. ) ;
#514 = CARTESIAN_POINT ( 'NONE',  ( 75.20570977803312473, 12.97982004111160315, 7.000000000000000000 ) ) ;
#515 = CARTESIAN_POINT ( 'NONE',  ( 0.5431871198829556491, -16.57708379306446389, 3.619024283482010329 ) ) ;
#516 = VERTEX_POINT ( 'NONE', #10650 ) ;
#517 = ORIENTED_EDGE ( 'NONE', *, *, #5979, .F. ) ;
#518 = CARTESIAN_POINT ( 'NONE',  ( 80.00000000000000000, 0.000000000000000000, -131.1575142076926852 ) ) ;
#519 = CARTESIAN_POINT ( 'NONE',  ( 2.790000000000061764, 5.211197193340692202, 13.21862218141517786 ) ) ;
#520 = EDGE_CURVE ( 'NONE', #3390, #5744, #103, .T. ) ;
#521 = ADVANCED_FACE ( 'NONE', ( #12728 ), #10775, .T. ) ;
#522 = B_SPLINE_CURVE_WITH_KNOTS ( 'NONE', 3,
 ( #4119, #4034, #8795, #7354, #2800, #7502 ),
 .UNSPECIFIED., .F., .F.,
 ( 4, 2, 4 ),
 ( 1.979325885420663221E-07, 0.001878588715165609505, 0.003756979497742676637 ),
 .UNSPECIFIED. ) ;
#523 = CYLINDRICAL_SURFACE ( 'NONE', #12954, 13.20000000000000107 ) ;
#524 = DIRECTION ( 'NONE',  ( -1.000000000000000000, -0.000000000000000000, -0.000000000000000000 ) ) ;
#525 = CARTESIAN_POINT ( 'NONE',  ( 1.394999999999999574, -4.147968289691484678, 27.76164181293050603 ) ) ;
#526 = VECTOR ( 'NONE', #5455, 1000.000000000000000 ) ;
#527 = CARTESIAN_POINT ( 'NONE',  ( 1.885839528871393611, 12.27244837507612729, 12.77651625388903511 ) ) ;
#528 = EDGE_LOOP ( 'NONE', ( #12850, #12024, #5679, #2607, #4048, #7554, #5899 ) ) ;
#529 = CARTESIAN_POINT ( 'NONE',  ( -5.209999999999999964, 0.000000000000000000, 0.000000000000000000 ) ) ;
#530 = B_SPLINE_CURVE_WITH_KNOTS ( 'NONE', 3,
 ( #8479, #3720, #8565, #2657 ),
 .UNSPECIFIED., .F., .F.,
 ( 4, 4 ),
 ( 0.005123695899043905454, 0.005814329666474870109 ),
 .UNSPECIFIED. ) ;
#531 = CARTESIAN_POINT ( 'NONE',  ( -9.403944755730117677, -13.79473832354794816, 22.00000000000000000 ) ) ;
#532 = ADVANCED_FACE ( 'NONE', ( #1053 ), #13021, .T. ) ;
#533 = SURFACE_STYLE_FILL_AREA ( #5103 ) ;
#534 = VECTOR ( 'NONE', #1828, 1000.000000000000000 ) ;
#535 = ORIENTED_EDGE ( 'NONE', *, *, #12540, .F. ) ;
#536 = ORIENTED_EDGE ( 'NONE', *, *, #9442, .F. ) ;
#537 = ORIENTED_EDGE ( 'NONE', *, *, #12943, .T. ) ;
#538 = CARTESIAN_POINT ( 'NONE',  ( 69.97572749000833880, 15.55805301486455683, 2.999999999999999112 ) ) ;
#539 = ADVANCED_FACE ( 'NONE', ( #8645 ), #1738, .T. ) ;
#540 = EDGE_CURVE ( 'NONE', #1061, #7151, #11199, .T. ) ;
#541 = ORIENTED_EDGE ( 'NONE', *, *, #8159, .F. ) ;
#542 = PRODUCT_DEFINITION_CONTEXT ( 'detailed design', #8310, 'design' ) ;
#543 = CYLINDRICAL_SURFACE ( 'NONE', #2690, 2.524999999999996358 ) ;
#544 = DIRECTION ( 'NONE',  ( -1.000000000000000000, 0.000000000000000000, 0.000000000000000000 ) ) ;
#545 = EDGE_CURVE ( 'NONE', #7272, #5145, #11103, .T. ) ;
#546 = VERTEX_POINT ( 'NONE', #8492 ) ;
#547 = VECTOR ( 'NONE', #3000, 1000.000000000000000 ) ;
#548 = LINE ( 'NONE', #11154, #9933 ) ;
#549 = CARTESIAN_POINT ( 'NONE',  ( 0.000000000000000000, 9.324097380959415204, 22.25075486061743391 ) ) ;
#550 = LINE ( 'NONE', #5266, #14058 ) ;
#551 = CARTESIAN_POINT ( 'NONE',  ( 0.000000000000000000, 9.324097380959777581, -22.25075486061729535 ) ) ;
#552 = VERTEX_POINT ( 'NONE', #6420 ) ;
#553 = CARTESIAN_POINT ( 'NONE',  ( 0.5537796329733288836, 16.15122426806996003, -5.139875429511683969 ) ) ;
#554 = CARTESIAN_POINT ( 'NONE',  ( 31.51081190520435626, 3.030430839836910639, 2.999999999999999112 ) ) ;
#555 = VERTEX_POINT ( 'NONE', #13184 ) ;
#556 = ORIENTED_EDGE ( 'NONE', *, *, #12002, .F. ) ;
#557 = CARTESIAN_POINT ( 'NONE',  ( 2.718131914667133220, -10.24630254990500511, -23.19485392143224445 ) ) ;
#558 = FILL_AREA_STYLE ('',( #14571 ) ) ;
#559 = CARTESIAN_POINT ( 'NONE',  ( 1.039999999999996039, 27.68468304288258963, 4.633866840649018215 ) ) ;
#560 = ADVANCED_FACE ( 'NONE', ( #7432 ), #3730, .T. ) ;
#561 = CARTESIAN_POINT ( 'NONE',  ( 2.765633920072238183, -18.55949924794904504, 16.37294372382852004 ) ) ;
#562 = ORIENTED_EDGE ( 'NONE', *, *, #11530, .T. ) ;
#563 = CARTESIAN_POINT ( 'NONE',  ( 2.236220367026669376, -5.139875429511969962, 16.15122426806987121 ) ) ;
#564 = CARTESIAN_POINT ( 'NONE',  ( 101.6227766016837819, -9.999999999999994671, 4.000000000000003553 ) ) ;
#565 = DIRECTION ( 'NONE',  ( -1.000000000000000000, 0.000000000000000000, 0.000000000000000000 ) ) ;
#566 =( NAMED_UNIT ( * ) SI_UNIT ( $, .STERADIAN. ) SOLID_ANGLE_UNIT ( ) );
#567 = VERTEX_POINT ( 'NONE', #338 ) ;
#568 = ORIENTED_EDGE ( 'NONE', *, *, #11623, .T. ) ;
#569 = PRODUCT_DEFINITION_FORMATION_WITH_SPECIFIED_SOURCE ( 'ANY', '', #11166, .NOT_KNOWN. ) ;
#570 = ORIENTED_EDGE ( 'NONE', *, *, #3691, .F. ) ;
#571 = CLOSED_SHELL ( 'NONE', ( #13465, #1305, #9432, #9490, #3541, #14835, #4258, #10117, #4020, #1002, #1343, #9186, #11729, #8337, #8823, #13143 ) ) ;
#572 = CARTESIAN_POINT ( 'NONE',  ( 0.1882239034349769691, -22.54313264455003463, -12.84621645676869939 ) ) ;
#573 = CARTESIAN_POINT ( 'NONE',  ( 1.039999999999996483, -19.67366047555544384, 20.02152543075338897 ) ) ;
#574 = EDGE_CURVE ( 'NONE', #4667, #7883, #12972, .T. ) ;
#575 = B_SPLINE_CURVE_WITH_KNOTS ( 'NONE', 3,
 ( #11221, #14616, #14475, #6311 ),
 .UNSPECIFIED., .F., .F.,
 ( 4, 4 ),
 ( 0.005258214619651938905, 0.005948481662034165590 ),
 .UNSPECIFIED. ) ;
#576 = AXIS2_PLACEMENT_3D ( 'NONE', #8107, #2415, #2263 ) ;
#577 = FACE_OUTER_BOUND ( 'NONE', #11814, .T. ) ;
#578 = VECTOR ( 'NONE', #11844, 1000.000000000000000 ) ;
#579 = CARTESIAN_POINT ( 'NONE',  ( 0.000000000000000000, 11.04103753892271733, 8.624777288397844188 ) ) ;
#580 = APPLICATION_PROTOCOL_DEFINITION ( 'draft international standard', 'automotive_design', 1998, #5084 ) ;
#581 = CARTESIAN_POINT ( 'NONE',  ( 0.4522159468065706789, -11.13074453164212407, 12.42068120944077236 ) ) ;
#582 = CARTESIAN_POINT ( 'NONE',  ( 80.00000000000000000, -9.999999999999994671, -130.1575142076926852 ) ) ;
#583 = DIRECTION ( 'NONE',  ( -1.000000000000000000, 0.000000000000000000, 0.000000000000000000 ) ) ;
#584 = ORIENTED_EDGE ( 'NONE', *, *, #6185, .F. ) ;
#585 = CARTESIAN_POINT ( 'NONE',  ( 83.50748565343083385, 13.38500995229612478, 7.000000000000000000 ) ) ;
#586 = FACE_OUTER_BOUND ( 'NONE', #1000, .T. ) ;
#587 = CIRCLE ( 'NONE', #5034, 28.06981291497571007 ) ;
#588 = DIRECTION ( 'NONE',  ( 0.000000000000000000, 0.000000000000000000, 1.000000000000000000 ) ) ;
#589 = EDGE_CURVE ( 'NONE', #6696, #11628, #955, .T. ) ;
#590 = ORIENTED_EDGE ( 'NONE', *, *, #386, .F. ) ;
#591 = CIRCLE ( 'NONE', #1085, 3.799999999999999378 ) ;
#592 = AXIS2_PLACEMENT_3D ( 'NONE', #283, #11969, #7217 ) ;
#593 = ADVANCED_FACE ( 'NONE', ( #8410 ), #2741, .F. ) ;
#594 = DIRECTION ( 'NONE',  ( 0.000000000000000000, 0.000000000000000000, -1.000000000000000000 ) ) ;
#595 = CARTESIAN_POINT ( 'NONE',  ( 0.000000000000000000, 0.000000000000000000, 0.000000000000000000 ) ) ;
#596 = ORIENTED_EDGE ( 'NONE', *, *, #3350, .T. ) ;
#597 = ORIENTED_EDGE ( 'NONE', *, *, #7976, .F. ) ;
#598 = CARTESIAN_POINT ( 'NONE',  ( -17.10144940350364706, -13.74829019802725050, -5.000000000000000000 ) ) ;
#599 = FACE_OUTER_BOUND ( 'NONE', #10458, .T. ) ;
#600 = CARTESIAN_POINT ( 'NONE',  ( 0.000000000000000000, 0.000000000000000000, 0.000000000000000000 ) ) ;
#601 = CARTESIAN_POINT ( 'NONE',  ( 0.5321745326902582729, -3.467596033028097935, -26.83036154824997510 ) ) ;
#602 = FACE_BOUND ( 'NONE', #4896, .T. ) ;
#603 = AXIS2_PLACEMENT_3D ( 'NONE', #6035, #9572, #1266 ) ;
#604 = AXIS2_PLACEMENT_3D ( 'NONE', #13155, #1321, #10708 ) ;
#605 = VECTOR ( 'NONE', #5620, 1000.000000000000114 ) ;
#606 = DIRECTION ( 'NONE',  ( 0.000000000000000000, 0.000000000000000000, 1.000000000000000000 ) ) ;
#607 = ORIENTED_EDGE ( 'NONE', *, *, #4698, .T. ) ;
#608 = CARTESIAN_POINT ( 'NONE',  ( 2.789999999999999147, -1.991882183130462503, 24.04302995059964942 ) ) ;
#609 = UNCERTAINTY_MEASURE_WITH_UNIT (LENGTH_MEASURE( 1.000000000000000082E-05 ), #10866, 'distance_accuracy_value', 'NONE');
#610 = PRODUCT_DEFINITION_SHAPE ( 'NONE', 'NONE',  #3183 ) ;
#611 = DIRECTION ( 'NONE',  ( 0.9863939238321437486, 0.1643989873053572359, -0.000000000000000000 ) ) ;
#612 = EDGE_CURVE ( 'NONE', #9447, #14273, #3176, .T. ) ;
#613 = VERTEX_POINT ( 'NONE', #6348 ) ;
#614 = AXIS2_PLACEMENT_3D ( 'NONE', #11477, #5656, #729 ) ;
#615 = CIRCLE ( 'NONE', #1363, 2.524999999999996358 ) ;
#616 =( GEOMETRIC_REPRESENTATION_CONTEXT ( 3 ) GLOBAL_UNCERTAINTY_ASSIGNED_CONTEXT ( ( #15080 ) ) GLOBAL_UNIT_ASSIGNED_CONTEXT ( ( #11232, #1944, #14708 ) ) REPRESENTATION_CONTEXT ( 'NONE', 'WORKASPACE' ) );
#617 = ORIENTED_EDGE ( 'NONE', *, *, #13935, .T. ) ;
#618 = ORIENTED_EDGE ( 'NONE', *, *, #1784, .F. ) ;
#619 = ORIENTED_EDGE ( 'NONE', *, *, #14712, .T. ) ;
#620 = CARTESIAN_POINT ( 'NONE',  ( 2.790000000000061764, -11.12234047011184046, -8.842064619038639606 ) ) ;
#621 = SURFACE_STYLE_USAGE ( .BOTH. , #11079 ) ;
#622 = EDGE_CURVE ( 'NONE', #7127, #13976, #12098, .T. ) ;
#623 = FACE_OUTER_BOUND ( 'NONE', #13605, .T. ) ;
#624 = DIRECTION ( 'NONE',  ( 0.000000000000000000, 0.000000000000000000, 1.000000000000000000 ) ) ;
#625 = AXIS2_PLACEMENT_3D ( 'NONE', #472, #6400, #14629 ) ;
#626 = VERTEX_POINT ( 'NONE', #4045 ) ;
#627 = CARTESIAN_POINT ( 'NONE',  ( 0.04914328897885022335, 13.98777112126087552, 5.263533129984400816 ) ) ;
#628 = CARTESIAN_POINT ( 'NONE',  ( 2.789999999999999147, 13.40591150984237245, -5.214906618939568084 ) ) ;
#629 = EDGE_CURVE ( 'NONE', #5767, #14821, #3491, .T. ) ;
#630 = EDGE_CURVE ( 'NONE', #7999, #6679, #7832, .T. ) ;
#631 = B_SPLINE_CURVE_WITH_KNOTS ( 'NONE', 3,
 ( #5423, #4332, #9013, #1871, #10017, #14718, #14636, #6404 ),
 .UNSPECIFIED., .F., .F.,
 ( 4, 2, 2, 4 ),
 ( 4.663089340421306733E-07, 0.001440500229357228462, 0.002160517189568826168, 0.002880534149780423873 ),
 .UNSPECIFIED. ) ;
#632 = DIRECTION ( 'NONE',  ( -1.000000000000000000, -0.000000000000000000, -0.000000000000000000 ) ) ;
#633 = CARTESIAN_POINT ( 'NONE',  ( 0.1882238946918236844, 2.857713464478689680, 25.78859396478529220 ) ) ;
#634 = CARTESIAN_POINT ( 'NONE',  ( 2.789999999999999147, -7.334849878007672963, 23.31896751603329676 ) ) ;
#635 = VERTEX_POINT ( 'NONE', #6124 ) ;
#636 = CARTESIAN_POINT ( 'NONE',  ( -0.1085714285714285687, -3.798448662927795372, -0.8000000000000000444 ) ) ;
#637 = TOROIDAL_SURFACE ( 'NONE', #8487, 24.12539914357697413, 8.000000000000000000 ) ;
#638 = CARTESIAN_POINT ( 'NONE',  ( 0.5321745407694743468, -26.58873630738047922, -4.993157874728098022 ) ) ;
#639 = ORIENTED_EDGE ( 'NONE', *, *, #11028, .T. ) ;
#640 = ORIENTED_EDGE ( 'NONE', *, *, #10463, .F. ) ;
#641 = STYLED_ITEM ( 'NONE', ( #131 ), #675 ) ;
#642 = DIRECTION ( 'NONE',  ( 0.000000000000000000, 0.000000000000000000, 1.000000000000000000 ) ) ;
#643 = DIRECTION ( 'NONE',  ( 0.000000000000000000, 0.5000000000000071054, -0.8660254037844345998 ) ) ;
#644 = CARTESIAN_POINT ( 'NONE',  ( 2.789999999999999147, 19.64056340710875048, 14.55412442567624609 ) ) ;
#645 = ADVANCED_FACE ( 'NONE', ( #2669 ), #12027, .F. ) ;
#646 = EDGE_CURVE ( 'NONE', #8930, #9867, #6269, .T. ) ;
#647 = AXIS2_PLACEMENT_3D ( 'NONE', #1933, #12597, #3237 ) ;
#648 = DIRECTION ( 'NONE',  ( 0.000000000000000000, 0.000000000000000000, 1.000000000000000000 ) ) ;
#649 = AXIS2_PLACEMENT_3D ( 'NONE', #720, #6335, #5200 ) ;
#651 = EDGE_LOOP ( 'NONE', ( #7645, #7888, #4599, #10882 ) ) ;
#650 = ADVANCED_FACE ( 'NONE', ( #7584 ), #3969, .T. ) ;
#652 = DIRECTION ( 'NONE',  ( 0.9148936170212769170, 0.4036950204470262649, 0.000000000000000000 ) ) ;
#653 = FACE_OUTER_BOUND ( 'NONE', #7548, .T. ) ;
#654 = AXIS2_PLACEMENT_3D ( 'NONE', #3244, #3311, #6925 ) ;
#655 = AXIS2_PLACEMENT_3D ( 'NONE', #13246, #8630, #13392 ) ;
#656 = ORIENTED_EDGE ( 'NONE', *, *, #11404, .T. ) ;
#657 = DIRECTION ( 'NONE',  ( -0.000000000000000000, -0.000000000000000000, -1.000000000000000000 ) ) ;
#658 = ORIENTED_EDGE ( 'NONE', *, *, #9106, .F. ) ;
#659 = ORIENTED_EDGE ( 'NONE', *, *, #7931, .T. ) ;
#660 = EDGE_CURVE ( 'NONE', #7996, #4412, #13722, .T. ) ;
#661 = CIRCLE ( 'NONE', #7295, 2.524999999999999023 ) ;
#662 = ORIENTED_EDGE ( 'NONE', *, *, #2587, .T. ) ;
#663 = CARTESIAN_POINT ( 'NONE',  ( 0.5321745227542320489, -18.57583492944406700, -19.66801664102725056 ) ) ;
#664 = DIRECTION ( 'NONE',  ( 0.000000000000000000, 0.000000000000000000, 1.000000000000000000 ) ) ;
#665 = DIRECTION ( 'NONE',  ( 0.000000000000000000, 0.000000000000000000, 1.000000000000000000 ) ) ;
#666 = PRODUCT_CONTEXT ( 'NONE', #2624, 'mechanical' ) ;
#667 = VECTOR ( 'NONE', #8814, 999.9999999999998863 ) ;
#668 = DIRECTION ( 'NONE',  ( -1.000000000000000000, 0.000000000000000000, -0.000000000000000000 ) ) ;
#669 = AXIS2_PLACEMENT_3D ( 'NONE', #2925, #13445, #8902 ) ;
#670 = DIRECTION ( 'NONE',  ( 0.000000000000000000, 0.000000000000000000, 1.000000000000000000 ) ) ;
#671 = DIRECTION ( 'NONE',  ( 0.000000000000000000, 0.000000000000000000, 1.000000000000000000 ) ) ;
#672 = VERTEX_POINT ( 'NONE', #7141 ) ;
#673 = CARTESIAN_POINT ( 'NONE',  ( 2.789999999999999147, 21.30679549418649543, -12.59161484032888723 ) ) ;
#674 = LINE ( 'NONE', #9057, #4725 ) ;
#675 = ADVANCED_BREP_SHAPE_REPRESENTATION ( '', ( #14111, #1376 ), #3356 ) ;
#676 = CARTESIAN_POINT ( 'NONE',  ( 2.781248467066446572, 13.40591150985955871, -5.214906618939568972 ) ) ;
#677 = VERTEX_POINT ( 'NONE', #4761 ) ;
#678 = MECHANICAL_DESIGN_GEOMETRIC_PRESENTATION_REPRESENTATION (  '', ( #1413 ), #6575 ) ;
#679 = DIRECTION ( 'NONE',  ( 1.000000000000000000, 0.000000000000000000, 0.000000000000000000 ) ) ;
#681 = TOROIDAL_SURFACE ( 'NONE', #3151, 4.100000000000000533, 0.1000000000000001582 ) ;
#680 = CARTESIAN_POINT ( 'NONE',  ( -0.1713913650100259145, 0.000000000000000000, 0.000000000000000000 ) ) ;
#682 = ORIENTED_EDGE ( 'NONE', *, *, #8049, .T. ) ;
#683 = AXIS2_PLACEMENT_3D ( 'NONE', #4148, #11052, #7449 ) ;
#684 = ORIENTED_EDGE ( 'NONE', *, *, #14154, .F. ) ;
#685 = EDGE_CURVE ( 'NONE', #7400, #10516, #10410, .T. ) ;
#686 = CARTESIAN_POINT ( 'NONE',  ( 4.000000000000000888, 4.898587196589413815E-16, 10.00000000000000000 ) ) ;
#687 = CARTESIAN_POINT ( 'NONE',  ( 0.007349557670560538138, -11.23191127083857133, -9.045126717605896260 ) ) ;
#688 = CARTESIAN_POINT ( 'NONE',  ( 0.5537796532149691364, -16.55730827443878539, -3.624349476775370782 ) ) ;
#689 = CARTESIAN_POINT ( 'NONE',  ( 0.02436607992776238310, -2.336989772644097574, -24.63872515616085224 ) ) ;
#690 = CARTESIAN_POINT ( 'NONE',  ( 0.000000000000000000, 24.04302995059966719, 1.991882183130389228 ) ) ;
#691 = CIRCLE ( 'NONE', #2900, 24.12539914357697768 ) ;
#692 = CARTESIAN_POINT ( 'NONE',  ( 2.789999999999999147, -7.739906618939802918, 13.40591150984224100 ) ) ;
#693 = LINE ( 'NONE', #9146, #14795 ) ;
#694 = ADVANCED_FACE ( 'NONE', ( #3381 ), #10531, .T. ) ;
#695 = ORIENTED_EDGE ( 'NONE', *, *, #5681, .F. ) ;
#696 = CARTESIAN_POINT ( 'NONE',  ( 0.02436607992776455150, -22.71065055754459650, 9.836394144775621129 ) ) ;
#697 = AXIS2_PLACEMENT_3D ( 'NONE', #7574, #6261, #2880 ) ;
#698 = AXIS2_PLACEMENT_3D ( 'NONE', #11572, #5829, #3434 ) ;
#699 = DIRECTION ( 'NONE',  ( 0.000000000000000000, 0.000000000000000000, 1.000000000000000000 ) ) ;
#700 = ORIENTED_EDGE ( 'NONE', *, *, #12767, .F. ) ;
#701 = SURFACE_SIDE_STYLE ('',( #2164 ) ) ;
#702 = ORIENTED_EDGE ( 'NONE', *, *, #8327, .F. ) ;
#703 = ORIENTED_EDGE ( 'NONE', *, *, #3534, .F. ) ;
#704 = ORIENTED_EDGE ( 'NONE', *, *, #12281, .T. ) ;
#705 = DIRECTION ( 'NONE',  ( -1.000000000000000000, 0.000000000000000000, -0.000000000000000000 ) ) ;
#706 = CARTESIAN_POINT ( 'NONE',  ( 2.030753610301994083, 19.12676442129372134, -19.86438386685639657 ) ) ;
#707 = AXIS2_PLACEMENT_3D ( 'NONE', #4857, #13219, #9532 ) ;
#708 = AXIS2_PLACEMENT_3D ( 'NONE', #5305, #9976, #14676 ) ;
#709 = CARTESIAN_POINT ( 'NONE',  ( 2.789999999999999147, -9.836394144775550075, -22.71065055754462492 ) ) ;
#710 = LINE ( 'NONE', #10011, #13396 ) ;
#711 = EDGE_CURVE ( 'NONE', #10374, #7184, #4924, .T. ) ;
#712 = ORIENTED_EDGE ( 'NONE', *, *, #3705, .T. ) ;
#713 = CYLINDRICAL_SURFACE ( 'NONE', #1338, 3.799999999999999378 ) ;
#714 = LINE ( 'NONE', #863, #6086 ) ;
#715 = LINE ( 'NONE', #4102, #2549 ) ;
#716 = ADVANCED_FACE ( 'NONE', ( #4624 ), #4697, .F. ) ;
#717 = AXIS2_PLACEMENT_3D ( 'NONE', #10345, #13964, #27 ) ;
#718 = DIRECTION ( 'NONE',  ( 1.445602896647338917E-16, -1.000000000000000000, 0.000000000000000000 ) ) ;
#719 = ORIENTED_EDGE ( 'NONE', *, *, #1592, .F. ) ;
#720 = CARTESIAN_POINT ( 'NONE',  ( 0.000000000000000000, 0.000000000000000000, 0.000000000000000000 ) ) ;
#721 = CARTESIAN_POINT ( 'NONE',  ( -1.000000000000000000, -6.008326913195983998, -0.8000000000000000444 ) ) ;
#722 = ORIENTED_EDGE ( 'NONE', *, *, #3716, .F. ) ;
#723 = ORIENTED_EDGE ( 'NONE', *, *, #13418, .T. ) ;
#724 = DIRECTION ( 'NONE',  ( 0.000000000000000000, 0.000000000000000000, 1.000000000000000000 ) ) ;
#725 = ADVANCED_FACE ( 'NONE', ( #9367 ), #12746, .F. ) ;
#726 = ADVANCED_FACE ( 'NONE', ( #10666 ), #6857, .T. ) ;
#727 = ADVANCED_FACE ( 'NONE', ( #4841 ), #15146, .T. ) ;
#728 = B_SPLINE_CURVE_WITH_KNOTS ( 'NONE', 3,
 ( #579, #5152, #8730, #13575 ),
 .UNSPECIFIED., .F., .F.,
 ( 4, 4 ),
 ( 0.005123695899043910658, 0.005814329666474866640 ),
 .UNSPECIFIED. ) ;
#729 = DIRECTION ( 'NONE',  ( 1.000000000000000000, 0.000000000000000000, 0.000000000000000000 ) ) ;
#730 = AXIS2_PLACEMENT_3D ( 'NONE', #2087, #9008, #2245 ) ;
#731 = EDGE_LOOP ( 'NONE', ( #12337, #9873, #12437, #11706, #9637 ) ) ;
#732 = B_SPLINE_CURVE_WITH_KNOTS ( 'NONE', 3,
 ( #13639, #6799, #14655, #14965, #5506, #14801 ),
 .UNSPECIFIED., .F., .F.,
 ( 4, 2, 4 ),
 ( 2.321268216996908089E-07, 0.001878622960950487733, 0.003757013795079275874 ),
 .UNSPECIFIED. ) ;
#733 = FACE_OUTER_BOUND ( 'NONE', #168, .T. ) ;
#734 = ORIENTED_EDGE ( 'NONE', *, *, #37, .F. ) ;
#735 = DIRECTION ( 'NONE',  ( 0.9021244663126475327, 0.4314758942051350465, -1.141265444721583757E-16 ) ) ;
#736 = DIRECTION ( 'NONE',  ( -5.782411586589355667E-16, -1.000000000000000000, 0.000000000000000000 ) ) ;
#737 = ORIENTED_EDGE ( 'NONE', *, *, #993, .F. ) ;
#738 = DIRECTION ( 'NONE',  ( 0.000000000000000000, 0.000000000000000000, 1.000000000000000000 ) ) ;
#739 = DIRECTION ( 'NONE',  ( 0.000000000000000000, 0.000000000000000000, -1.000000000000000000 ) ) ;
#740 = ORIENTED_EDGE ( 'NONE', *, *, #1383, .F. ) ;
#741 = AXIS2_PLACEMENT_3D ( 'NONE', #2504, #7190, #11721 ) ;
#742 = EDGE_CURVE ( 'NONE', #7471, #6879, #3519, .T. ) ;
#743 = ORIENTED_EDGE ( 'NONE', *, *, #8518, .T. ) ;
#744 = FACE_OUTER_BOUND ( 'NONE', #8998, .T. ) ;
#745 = FACE_OUTER_BOUND ( 'NONE', #3548, .T. ) ;
#746 = ADVANCED_FACE ( 'NONE', ( #2228 ), #6914, .F. ) ;
#747 = CARTESIAN_POINT ( 'NONE',  ( -4.000000000000000000, 0.000000000000000000, 6.000000000000000000 ) ) ;
#748 = CARTESIAN_POINT ( 'NONE',  ( 2.789999999999999147, -24.34211360614305875, 7.909232158574721616 ) ) ;
#749 = CARTESIAN_POINT ( 'NONE',  ( 50.00050000000000239, 4.898587196589412829E-16, -4.000000000000000000 ) ) ;
#750 = FACE_OUTER_BOUND ( 'NONE', #10103, .T. ) ;
#751 = DIRECTION ( 'NONE',  ( 0.000000000000000000, 0.000000000000000000, 1.000000000000000000 ) ) ;
#752 = EDGE_CURVE ( 'NONE', #10751, #2037, #9519, .T. ) ;
#753 = EDGE_LOOP ( 'NONE', ( #1969, #1811, #5274, #1615 ) ) ;
#754 = CARTESIAN_POINT ( 'NONE',  ( 2.764680872515352217, 2.311161484776756758, -14.46287784598614756 ) ) ;
#755 = DIRECTION ( 'NONE',  ( -1.000000000000000000, 0.000000000000000000, 0.000000000000000000 ) ) ;
#756 = CARTESIAN_POINT ( 'NONE',  ( -15.94493884710238696, -7.321218896460230496, -3.800000000000000266 ) ) ;
#757 = B_SPLINE_CURVE_WITH_KNOTS ( 'NONE', 3,
 ( #2681, #12103, #1282, #5975 ),
 .UNSPECIFIED., .F., .F.,
 ( 4, 4 ),
 ( 0.005123742438166214823, 0.005814376014856804595 ),
 .UNSPECIFIED. ) ;
#758 = ORIENTED_EDGE ( 'NONE', *, *, #5172, .T. ) ;
#759 = FACE_OUTER_BOUND ( 'NONE', #2011, .T. ) ;
#760 = DIRECTION ( 'NONE',  ( 0.02857142857142857401, 0.9995917534020515305, -0.000000000000000000 ) ) ;
#761 = VERTEX_POINT ( 'NONE', #8286 ) ;
#762 = ORIENTED_EDGE ( 'NONE', *, *, #12185, .F. ) ;
#763 = CYLINDRICAL_SURFACE ( 'NONE', #4849, 28.06981291497571362 ) ;
#764 = FACE_OUTER_BOUND ( 'NONE', #9154, .T. ) ;
#765 = CARTESIAN_POINT ( 'NONE',  ( 2.764680872515352217, 2.311161484776756758, -14.46287784598614756 ) ) ;
#766 = DIRECTION ( 'NONE',  ( 0.000000000000000000, 1.374038396813314756E-15, -1.000000000000000000 ) ) ;
#767 = DIRECTION ( 'NONE',  ( -1.000000000000000000, -0.000000000000000000, -0.000000000000000000 ) ) ;
#768 = CYLINDRICAL_SURFACE ( 'NONE', #12984, 8.400000000000000355 ) ;
#769 = DIRECTION ( 'NONE',  ( -0.9863939238321437486, -0.1643989873053574857, 0.000000000000000000 ) ) ;
#770 = ORIENTED_EDGE ( 'NONE', *, *, #10353, .F. ) ;
#771 = CARTESIAN_POINT ( 'NONE',  ( -7.755480735455585059E-14, 24.22524813288762502, -2.133839912090887303 ) ) ;
#772 = DIRECTION ( 'NONE',  ( 0.000000000000000000, -1.000000000000000000, 0.000000000000000000 ) ) ;
#773 = ORIENTED_EDGE ( 'NONE', *, *, #13006, .T. ) ;
#774 = ORIENTED_EDGE ( 'NONE', *, *, #12921, .T. ) ;
#775 = ORIENTED_EDGE ( 'NONE', *, *, #109, .T. ) ;
#776 = ORIENTED_EDGE ( 'NONE', *, *, #5121, .F. ) ;
#777 = DIRECTION ( 'NONE',  ( 0.000000000000000000, 0.000000000000000000, 1.000000000000000000 ) ) ;
#778 = PRESENTATION_STYLE_ASSIGNMENT (( #621 ) ) ;
#779 = EDGE_CURVE ( 'NONE', #11305, #1805, #11744, .T. ) ;
#780 = LINE ( 'NONE', #13773, #10301 ) ;
#781 = ORIENTED_EDGE ( 'NONE', *, *, #7792, .F. ) ;
#782 = LINE ( 'NONE', #2247, #5291 ) ;
#783 = DIRECTION ( 'NONE',  ( 0.000000000000000000, 0.8660254037844327124, 0.5000000000000104361 ) ) ;
#784 = CARTESIAN_POINT ( 'NONE',  ( -14.40394475573011945, -10.79473832354794460, -3.469446951953614189E-15 ) ) ;
#785 = AXIS2_PLACEMENT_3D ( 'NONE', #4746, #10427, #14110 ) ;
#786 = DIRECTION ( 'NONE',  ( -1.000000000000000000, -0.000000000000000000, -0.000000000000000000 ) ) ;
#787 = ADVANCED_FACE ( 'NONE', ( #11592 ), #14342, .T. ) ;
#788 = ORIENTED_EDGE ( 'NONE', *, *, #5470, .F. ) ;
#789 = CARTESIAN_POINT ( 'NONE',  ( 2.789999999999999147, 2.680914349914567470E-13, -25.59481291497571220 ) ) ;
#790 = EDGE_CURVE ( 'NONE', #6334, #6870, #7715, .T. ) ;
#791 = CARTESIAN_POINT ( 'NONE',  ( 4.000000000000000000, 4.898587196589412829E-16, 3.895000000000000462 ) ) ;
#792 = ORIENTED_EDGE ( 'NONE', *, *, #2442, .T. ) ;
#793 = ORIENTED_EDGE ( 'NONE', *, *, #2254, .F. ) ;
#794 = AXIS2_PLACEMENT_3D ( 'NONE', #9301, #8135, #991 ) ;
#795 = EDGE_CURVE ( 'NONE', #10796, #2610, #10470, .T. ) ;
#796 = CARTESIAN_POINT ( 'NONE',  ( 0.02436607992776151574, -16.37294372382871188, 18.55949924794887096 ) ) ;
#797 = VERTEX_POINT ( 'NONE', #2296 ) ;
#798 = CARTESIAN_POINT ( 'NONE',  ( 1.039999999999998037, -4.835383649608592904, 17.29145405592687368 ) ) ;
#799 = VERTEX_POINT ( 'NONE', #7292 ) ;
#800 = CARTESIAN_POINT ( 'NONE',  ( 59.43001430450886602, 34.23215029930534570, -8.169391093593850073 ) ) ;
#801 = CARTESIAN_POINT ( 'NONE',  ( 0.000000000000000000, 15.74360496233383522, 18.28042085475283329 ) ) ;
#802 = ORIENTED_EDGE ( 'NONE', *, *, #10049, .T. ) ;
#803 = CARTESIAN_POINT ( 'NONE',  ( 2.601776096565022289, 12.84621645676845070, 22.54313264455018384 ) ) ;
#804 = EDGE_CURVE ( 'NONE', #11628, #8517, #3296, .T. ) ;
#805 = AXIS2_PLACEMENT_3D ( 'NONE', #9265, #4731, #5810 ) ;
#806 = ORIENTED_EDGE ( 'NONE', *, *, #13764, .F. ) ;
#807 = VERTEX_POINT ( 'NONE', #12276 ) ;
#808 = ORIENTED_EDGE ( 'NONE', *, *, #12374, .T. ) ;
#809 = FILL_AREA_STYLE_COLOUR ( '', #12455 ) ;
#810 = CARTESIAN_POINT ( 'NONE',  ( 2.789999999999999147, -14.55412442567631537, 19.64056340710869719 ) ) ;
#811 = ADVANCED_FACE ( 'NONE', ( #2827 ), #9663, .F. ) ;
#812 = CYLINDRICAL_SURFACE ( 'NONE', #5102, 4.000000000000000000 ) ;
#813 = CARTESIAN_POINT ( 'NONE',  ( -3.510166481118844661, -1.455586230640303347, -7.000000000000007994 ) ) ;
#814 = APPLICATION_PROTOCOL_DEFINITION ( 'draft international standard', 'automotive_design', 1998, #3121 ) ;
#815 = CARTESIAN_POINT ( 'NONE',  ( 2.789999999999999147, 20.70663861606293210, -15.04425356660737556 ) ) ;
#816 = CARTESIAN_POINT ( 'NONE',  ( 0.000000000000000000, -15.74360496233395956, 18.28042085475273026 ) ) ;
#817 = EDGE_CURVE ( 'NONE', #7184, #9117, #7348, .T. ) ;
#818 = ORIENTED_EDGE ( 'NONE', *, *, #10308, .T. ) ;
#819 = DIRECTION ( 'NONE',  ( 1.000000000000000000, 1.445602896647338424E-16, 0.000000000000000000 ) ) ;
#820 = LINE ( 'NONE', #13660, #10113 ) ;
#821 = LINE ( 'NONE', #8895, #898 ) ;
#822 = ADVANCED_FACE ( 'NONE', ( #357 ), #14285, .F. ) ;
#823 = EDGE_CURVE ( 'NONE', #14366, #10930, #6243, .T. ) ;
#824 = AXIS2_PLACEMENT_3D ( 'NONE', #2453, #1360, #7373 ) ;
#825 = ORIENTED_EDGE ( 'NONE', *, *, #12060, .T. ) ;
#826 = B_SPLINE_CURVE_WITH_KNOTS ( 'NONE', 3,
 ( #8174, #2337, #1325, #5806 ),
 .UNSPECIFIED., .F., .F.,
 ( 4, 4 ),
 ( 0.005258214619651955385, 0.005948481662034169927 ),
 .UNSPECIFIED. ) ;
#827 = DIRECTION ( 'NONE',  ( -1.000000000000000000, -0.000000000000000000, 0.000000000000000000 ) ) ;
#828 = LINE ( 'NONE', #2218, #7522 ) ;
#829 = ORIENTED_EDGE ( 'NONE', *, *, #13134, .T. ) ;
#830 = ORIENTED_EDGE ( 'NONE', *, *, #14959, .F. ) ;
#831 = B_SPLINE_CURVE_WITH_KNOTS ( 'NONE', 3,
 ( #2977, #1985, #13577, #581, #6511, #13738, #7665, #6669 ),
 .UNSPECIFIED., .F., .F.,
 ( 4, 2, 2, 4 ),
 ( 2.445728210282456254E-07, 0.001895260649874687007, 0.002842768688401519240, 0.003790276726928351256 ),
 .UNSPECIFIED. ) ;
#832 = DIRECTION ( 'NONE',  ( -1.000000000000000000, 0.000000000000000000, 0.000000000000000000 ) ) ;
#833 = DIRECTION ( 'NONE',  ( -1.000000000000000000, 0.000000000000000000, 0.000000000000000000 ) ) ;
#834 = ORIENTED_EDGE ( 'NONE', *, *, #13052, .F. ) ;
#835 = CARTESIAN_POINT ( 'NONE',  ( 2.031033465052725084, -4.828387785248216879, 27.14933624560906367 ) ) ;
#836 = CARTESIAN_POINT ( 'NONE',  ( -2.141980652367355020, -6.189445006155633422, 0.000000000000000000 ) ) ;
#837 = DIRECTION ( 'NONE',  ( 0.000000000000000000, 0.000000000000000000, 1.000000000000000000 ) ) ;
#838 = FACE_OUTER_BOUND ( 'NONE', #3603, .T. ) ;
#839 = CARTESIAN_POINT ( 'NONE',  ( 2.765633920072236407, 2.336989772644613161, -24.63872515616080250 ) ) ;
#840 = EDGE_CURVE ( 'NONE', #14323, #9602, #11010, .T. ) ;
#841 = AXIS2_PLACEMENT_3D ( 'NONE', #8446, #219, #11761 ) ;
#842 = EDGE_CURVE ( 'NONE', #85, #7278, #10281, .T. ) ;
#843 = ORIENTED_EDGE ( 'NONE', *, *, #13220, .F. ) ;
#844 = FACE_OUTER_BOUND ( 'NONE', #4156, .T. ) ;
#845 = VECTOR ( 'NONE', #12005, 1000.000000000000000 ) ;
#846 = VECTOR ( 'NONE', #7852, 1000.000000000000000 ) ;
#847 = CARTESIAN_POINT ( 'NONE',  ( 8.000000000000000000, 0.000000000000000000, 0.000000000000000000 ) ) ;
#848 = ADVANCED_FACE ( 'NONE', ( #7599 ), #15085, .T. ) ;
#849 = ORIENTED_EDGE ( 'NONE', *, *, #4788, .T. ) ;
#850 = ORIENTED_EDGE ( 'NONE', *, *, #1681, .T. ) ;
#851 = VERTEX_POINT ( 'NONE', #7377 ) ;
#852 = VERTEX_POINT ( 'NONE', #6139 ) ;
#853 = CARTESIAN_POINT ( 'NONE',  ( 2.597943782557557313, -12.05486625177578830, 10.28947301956278082 ) ) ;
#854 = AXIS2_PLACEMENT_3D ( 'NONE', #10836, #10689, #6078 ) ;
#855 = AXIS2_PLACEMENT_3D ( 'NONE', #5788, #13776, #8092 ) ;
#856 = CARTESIAN_POINT ( 'NONE',  ( 0.02436607992775544421, -22.71065055754445439, -9.836394144775947979 ) ) ;
#857 = ADVANCED_FACE ( 'NONE', ( #3913 ), #278, .F. ) ;
#858 = TOROIDAL_SURFACE ( 'NONE', #3786, 24.12539914357697413, 8.000000000000000000 ) ;
#859 = LINE ( 'NONE', #13924, #966 ) ;
#860 = VERTEX_POINT ( 'NONE', #8511 ) ;
#861 = DIRECTION ( 'NONE',  ( 0.000000000000000000, 0.000000000000000000, 1.000000000000000000 ) ) ;
#862 = FACE_OUTER_BOUND ( 'NONE', #14868, .T. ) ;
#863 = CARTESIAN_POINT ( 'NONE',  ( 31.51081190520435626, 3.030430839836910639, 2.999999999999999112 ) ) ;
#864 = AXIS2_PLACEMENT_3D ( 'NONE', #2501, #3652, #7037 ) ;
#865 = AXIS2_PLACEMENT_3D ( 'NONE', #4110, #8790, #13481 ) ;
#866 = CARTESIAN_POINT ( 'NONE',  ( 0.1570303611602991700, -22.37100459959352605, 12.81671916049007365 ) ) ;
#867 = ORIENTED_EDGE ( 'NONE', *, *, #10936, .T. ) ;
#868 = DIRECTION ( 'NONE',  ( 0.000000000000000000, 0.000000000000000000, -1.000000000000000000 ) ) ;
#869 = CARTESIAN_POINT ( 'NONE',  ( 0.02436607992775978102, -12.59161484032896361, -21.30679549418645280 ) ) ;
#870 = ORIENTED_EDGE ( 'NONE', *, *, #10742, .T. ) ;
#871 = ORIENTED_EDGE ( 'NONE', *, *, #5784, .F. ) ;
#872 = VECTOR ( 'NONE', #5496, 1000.000000000000000 ) ;
#873 = DIRECTION ( 'NONE',  ( 0.1643989873053570416, -0.9863939238321438596, 0.000000000000000000 ) ) ;
#874 = ORIENTED_EDGE ( 'NONE', *, *, #399, .F. ) ;
#875 = CYLINDRICAL_SURFACE ( 'NONE', #11476, 13.19999999999999929 ) ;
#876 = EDGE_CURVE ( 'NONE', #4522, #1158, #13844, .T. ) ;
#877 = ORIENTED_EDGE ( 'NONE', *, *, #7016, .T. ) ;
#878 = CARTESIAN_POINT ( 'NONE',  ( -9.999999999999998224, 0.000000000000000000, -131.1575142076926852 ) ) ;
#879 = CARTESIAN_POINT ( 'NONE',  ( 2.789999999999999147, -24.34211360614305875, 7.909232158574721616 ) ) ;
#880 = ORIENTED_EDGE ( 'NONE', *, *, #7600, .T. ) ;
#881 = VECTOR ( 'NONE', #2943, 1000.000000000000000 ) ;
#882 = CARTESIAN_POINT ( 'NONE',  ( 0.02531912748464848137, 2.311161484776556030, 14.46287784598618309 ) ) ;
#883 = VERTEX_POINT ( 'NONE', #14448 ) ;
#884 = ORIENTED_EDGE ( 'NONE', *, *, #9768, .T. ) ;
#885 = SURFACE_STYLE_FILL_AREA ( #6505 ) ;
#886 = CARTESIAN_POINT ( 'NONE',  ( 2.789999999999999147, 24.04302995059966364, -1.991882183130384121 ) ) ;
#887 = DIRECTION ( 'NONE',  ( -1.000000000000000000, -0.000000000000000000, -0.000000000000000000 ) ) ;
#888 = CARTESIAN_POINT ( 'NONE',  ( 0.8291131470075423504, 24.44424927289185945, 12.96989951879416125 ) ) ;
#889 = B_SPLINE_CURVE_WITH_KNOTS ( 'NONE', 3,
 ( #3132, #1814, #6729, #14972 ),
 .UNSPECIFIED., .F., .F.,
 ( 4, 4 ),
 ( 2.159563976372915910E-07, 0.0006916893629248579154 ),
 .UNSPECIFIED. ) ;
#890 = LINE ( 'NONE', #749, #1286 ) ;
#891 = AXIS2_PLACEMENT_3D ( 'NONE', #7418, #1421, #10719 ) ;
#892 = CARTESIAN_POINT ( 'NONE',  ( 2.789679245949058917, 20.70663861606308487, -12.51925356660738053 ) ) ;
#893 = CIRCLE ( 'NONE', #11692, 4.000000000000000888 ) ;
#894 = ORIENTED_EDGE ( 'NONE', *, *, #14558, .T. ) ;
#895 = DIRECTION ( 'NONE',  ( -1.000000000000000000, -0.000000000000000000, -0.000000000000000000 ) ) ;
#896 = CARTESIAN_POINT ( 'NONE',  ( 1.394999999999999574, 4.633866840649313090, -27.68468304288253989 ) ) ;
#897 = CARTESIAN_POINT ( 'NONE',  ( 3.751931928061364552, -0.6025004624012525456, 7.799999999999990052 ) ) ;
#898 = VECTOR ( 'NONE', #12581, 1000.000000000000000 ) ;
#899 = CIRCLE ( 'NONE', #10472, 24.12539914357697413 ) ;
#900 = ORIENTED_EDGE ( 'NONE', *, *, #3910, .F. ) ;
#901 = EDGE_CURVE ( 'NONE', #14849, #9696, #2754, .T. ) ;
#902 = DIRECTION ( 'NONE',  ( -1.000000000000000000, -0.000000000000000000, -0.000000000000000000 ) ) ;
#903 = DIRECTION ( 'NONE',  ( -0.000000000000000000, 0.000000000000000000, 1.000000000000000000 ) ) ;
#904 = EDGE_LOOP ( 'NONE', ( #11080, #1437, #4193, #4487 ) ) ;
#905 = AXIS2_PLACEMENT_3D ( 'NONE', #10833, #8147, #8369 ) ;
#906 = EDGE_LOOP ( 'NONE', ( #12011, #939, #11934, #6137, #14725, #5584 ) ) ;
#907 = AXIS2_PLACEMENT_3D ( 'NONE', #8503, #6206, #13195 ) ;
#908 = DIRECTION ( 'NONE',  ( 0.000000000000000000, 0.000000000000000000, 1.000000000000000000 ) ) ;
#909 = LINE ( 'NONE', #10292, #5851 ) ;
#910 = VERTEX_POINT ( 'NONE', #9890 ) ;
#911 = DIRECTION ( 'NONE',  ( 0.000000000000000000, 0.000000000000000000, -1.000000000000000000 ) ) ;
#912 = DIRECTION ( 'NONE',  ( -1.000000000000000000, -0.000000000000000000, -0.000000000000000000 ) ) ;
#913 = LINE ( 'NONE', #4463, #605 ) ;
#914 = EDGE_CURVE ( 'NONE', #9975, #4099, #3982, .T. ) ;
#915 = EDGE_CURVE ( 'NONE', #3460, #13819, #8735, .T. ) ;
#916 = AXIS2_PLACEMENT_3D ( 'NONE', #8393, #86, #2266 ) ;
#917 = ADVANCED_FACE ( 'NONE', ( #15187 ), #1318, .T. ) ;
#918 = CARTESIAN_POINT ( 'NONE',  ( 0.1855657168891864939, -12.84444904262008436, -22.53097606932998787 ) ) ;
#919 = CARTESIAN_POINT ( 'NONE',  ( 72.68384697807672978, 11.35494834827056110, -2.000000000000000888 ) ) ;
#920 = ORIENTED_EDGE ( 'NONE', *, *, #6461, .F. ) ;
#921 = CARTESIAN_POINT ( 'NONE',  ( 0.1717365941144614605, -6.008326913195983998, -0.8000000000000000444 ) ) ;
#922 = CIRCLE ( 'NONE', #14681, 24.12539914357697768 ) ;
#923 = CARTESIAN_POINT ( 'NONE',  ( -16.14082873121598993, -7.414910804916202913, -3.000000000000000000 ) ) ;
#924 = CIRCLE ( 'NONE', #3389, 2.000000000000003109 ) ;
#925 = ORIENTED_EDGE ( 'NONE', *, *, #3499, .F. ) ;
#926 = AXIS2_PLACEMENT_3D ( 'NONE', #8242, #7946, #12629 ) ;
#927 = ORIENTED_EDGE ( 'NONE', *, *, #12743, .T. ) ;
#928 = EDGE_LOOP ( 'NONE', ( #1613, #4528 ) ) ;
#929 = VERTEX_POINT ( 'NONE', #11555 ) ;
#930 = ADVANCED_FACE ( 'NONE', ( #12777 ), #3415, .T. ) ;
#931 = DIRECTION ( 'NONE',  ( 1.000000000000000000, 0.000000000000000000, 0.000000000000000000 ) ) ;
#932 = EDGE_CURVE ( 'NONE', #12029, #4099, #5029, .T. ) ;
#933 = DIRECTION ( 'NONE',  ( 0.000000000000000000, 0.000000000000000000, 1.000000000000000000 ) ) ;
#934 = CIRCLE ( 'NONE', #4638, 28.06981291497571362 ) ;
#935 = CARTESIAN_POINT ( 'NONE',  ( 2.697960317788776763, -5.280991956247018670, -14.31435947614547821 ) ) ;
#936 = EDGE_CURVE ( 'NONE', #4803, #367, #12085, .T. ) ;
#937 = CIRCLE ( 'NONE', #9527, 4.000000000000003553 ) ;
#938 = CARTESIAN_POINT ( 'NONE',  ( 2.604434283110813375, -12.84444904262041121, 22.53097606932980312 ) ) ;
#939 = ORIENTED_EDGE ( 'NONE', *, *, #14144, .F. ) ;
#940 = CARTESIAN_POINT ( 'NONE',  ( 2.781248467067199748, -13.40591150984217705, -5.214906618939849636 ) ) ;
#941 = CARTESIAN_POINT ( 'NONE',  ( -1.149999999999998135, 5.021051876504148371E-16, 4.100000000000000533 ) ) ;
#942 = EDGE_CURVE ( 'NONE', #3736, #15013, #2794, .T. ) ;
#943 = CARTESIAN_POINT ( 'NONE',  ( 1.387778780781445676E-14, 0.000000000000000000, -7.800000000000008704 ) ) ;
#944 = CIRCLE ( 'NONE', #2663, 0.7500000000000002220 ) ;
#945 = AXIS2_PLACEMENT_3D ( 'NONE', #5676, #3219, #1827 ) ;
#946 = ORIENTED_EDGE ( 'NONE', *, *, #10600, .T. ) ;
#947 = DIRECTION ( 'NONE',  ( 0.000000000000000000, 0.000000000000000000, -1.000000000000000000 ) ) ;
#948 = CARTESIAN_POINT ( 'NONE',  ( 67.23404255319148604, 28.93147646537027384, -130.1575142076926852 ) ) ;
#949 = VERTEX_POINT ( 'NONE', #7667 ) ;
#950 = ORIENTED_EDGE ( 'NONE', *, *, #6665, .T. ) ;
#951 = CARTESIAN_POINT ( 'NONE',  ( 0.1999999999999985678, -6.997142273814360713, -0.8000000000000000444 ) ) ;
#952 = VERTEX_POINT ( 'NONE', #6947 ) ;
#953 = DIRECTION ( 'NONE',  ( 1.000000000000000000, 0.000000000000000000, 0.000000000000000000 ) ) ;
#954 =( REPRESENTATION_RELATIONSHIP ('NONE','NONE', #12685, #5737 ) REPRESENTATION_RELATIONSHIP_WITH_TRANSFORMATION ( #2350 )SHAPE_REPRESENTATION_RELATIONSHIP( ) );
#955 = CIRCLE ( 'NONE', #5146, 2.524999999999995470 ) ;
#956 = AXIS2_PLACEMENT_3D ( 'NONE', #3416, #10487, #78 ) ;
#957 = TOROIDAL_SURFACE ( 'NONE', #14218, 14.01039946648073986, 8.000000000000000000 ) ;
#958 = DIRECTION ( 'NONE',  ( -1.000000000000000000, -0.000000000000000000, -0.000000000000000000 ) ) ;
#959 = CARTESIAN_POINT ( 'NONE',  ( -5.209999999999999964, 0.000000000000000000, 0.000000000000000000 ) ) ;
#960 = VERTEX_POINT ( 'NONE', #10398 ) ;
#961 =( LENGTH_UNIT ( ) NAMED_UNIT ( * ) SI_UNIT ( .MILLI., .METRE. ) );
#962 = CARTESIAN_POINT ( 'NONE',  ( -0.4472135954999577612, 5.633375276077824112E-16, 4.599999999999999645 ) ) ;
#963 = EDGE_LOOP ( 'NONE', ( #14010, #3340, #770, #13005 ) ) ;
#964 = ORIENTED_EDGE ( 'NONE', *, *, #62, .F. ) ;
#965 = CARTESIAN_POINT ( 'NONE',  ( 2.262072661820536901, 3.461047254864260125, 26.82026385750179287 ) ) ;
#966 = VECTOR ( 'NONE', #4326, 1000.000000000000000 ) ;
#967 = CARTESIAN_POINT ( 'NONE',  ( 2.789999999999999147, -5.404747904883309660E-14, 15.47981323787947794 ) ) ;
#968 = DIRECTION ( 'NONE',  ( 0.000000000000000000, -1.000000000000000000, 0.000000000000000000 ) ) ;
#969 = CARTESIAN_POINT ( 'NONE',  ( -1.250000000000001110, 0.000000000000000000, -5.575000000000000178 ) ) ;
#970 = CONTEXT_DEPENDENT_SHAPE_REPRESENTATION ( #1744, #13881 ) ;
#971 = CARTESIAN_POINT ( 'NONE',  ( 2.789999999999999147, 13.87420763704361093, 1.948757464274220697 ) ) ;
#972 = EDGE_CURVE ( 'NONE', #6697, #12699, #13604, .T. ) ;
#973 = CARTESIAN_POINT ( 'NONE',  ( 2.718131864678288601, -25.22589920183363432, 2.577209017046923289 ) ) ;
#974 = ORIENTED_EDGE ( 'NONE', *, *, #2510, .F. ) ;
#975 = CARTESIAN_POINT ( 'NONE',  ( 31.51081190520435626, 3.030430839836910639, 4.000000000000000000 ) ) ;
#976 = DIRECTION ( 'NONE',  ( -1.000000000000000000, 0.000000000000000000, 0.000000000000000000 ) ) ;
#977 = VECTOR ( 'NONE', #5224, 1000.000000000000000 ) ;
#978 = CARTESIAN_POINT ( 'NONE',  ( 0.02531912748631078014, -2.311161484776655950, 14.46287784598616355 ) ) ;
#979 = ORIENTED_EDGE ( 'NONE', *, *, #5847, .F. ) ;
#980 = EDGE_CURVE ( 'NONE', #11004, #15169, #15103, .T. ) ;
#981 = CARTESIAN_POINT ( 'NONE',  ( 15.21482963846748504, 16.90833299098317610, 3.000000000000002665 ) ) ;
#982 = DIRECTION ( 'NONE',  ( 0.000000000000000000, 0.000000000000000000, -1.000000000000000000 ) ) ;
#983 = ORIENTED_EDGE ( 'NONE', *, *, #14788, .T. ) ;
#984 = ORIENTED_EDGE ( 'NONE', *, *, #4943, .F. ) ;
#985 = CARTESIAN_POINT ( 'NONE',  ( 0.2818303916520940589, 5.259531939870414341, -15.25429862889476240 ) ) ;
#986 = CARTESIAN_POINT ( 'NONE',  ( 1.394999999999999574, 20.02152543075346003, 19.67366047555537634 ) ) ;
#987 = EDGE_CURVE ( 'NONE', #4130, #12548, #3711, .T. ) ;
#988 = VERTEX_POINT ( 'NONE', #5302 ) ;
#989 = CARTESIAN_POINT ( 'NONE',  ( 2.262072625383133140, -4.996265754456554298, 26.57710921259759829 ) ) ;
#990 = CARTESIAN_POINT ( 'NONE',  ( 0.006930995026450116094, -5.408431875071277872, -23.92277630352801054 ) ) ;
#991 = DIRECTION ( 'NONE',  ( -1.000000000000000000, 0.000000000000000000, -0.000000000000000000 ) ) ;
#992 = B_SPLINE_CURVE_WITH_KNOTS ( 'NONE', 3,
 ( #4190, #6566, #9941, #3027, #5427, #7643, #7714, #5497 ),
 .UNSPECIFIED., .F., .F.,
 ( 4, 2, 2, 4 ),
 ( 4.663089536290197543E-07, 0.001898630414085408650, 0.002847712466651295803, 0.003796794519217183174 ),
 .UNSPECIFIED. ) ;
#993 = EDGE_CURVE ( 'NONE', #5463, #635, #14081, .T. ) ;
#994 = DIRECTION ( 'NONE',  ( 1.000000000000000000, 0.000000000000000000, 0.000000000000000000 ) ) ;
#995 = LINE ( 'NONE', #4236, #547 ) ;
#996 = ORIENTED_EDGE ( 'NONE', *, *, #9649, .F. ) ;
#997 = CARTESIAN_POINT ( 'NONE',  ( 0.02436607992775978102, 24.63872515616082737, 2.336989772644355146 ) ) ;
#998 = PRODUCT_DEFINITION_SHAPE ( 'NONE', 'NONE',  #15224 ) ;
#999 = DIRECTION ( 'NONE',  ( -1.000000000000000000, -0.000000000000000000, -0.000000000000000000 ) ) ;
#1000 = EDGE_LOOP ( 'NONE', ( #10311, #6178, #2088, #10360 ) ) ;
#1001 = B_SPLINE_CURVE_WITH_KNOTS ( 'NONE', 3,
 ( #1140, #4615, #14043, #11654 ),
 .UNSPECIFIED., .F., .F.,
 ( 4, 4 ),
 ( 0.0002742066915202718549, 0.0006916721208754016484 ),
 .UNSPECIFIED. ) ;
#1002 = ADVANCED_FACE ( 'NONE', ( #5726 ), #2188, .F. ) ;
#1003 = FILL_AREA_STYLE ('',( #7855 ) ) ;
#1004 = ADVANCED_FACE ( 'NONE', ( #1031 ), #8438, .T. ) ;
#1005 = ORIENTED_EDGE ( 'NONE', *, *, #4117, .F. ) ;
#1006 = ORIENTED_EDGE ( 'NONE', *, *, #3006, .F. ) ;
#1007 = VERTEX_POINT ( 'NONE', #9258 ) ;
#1008 = CARTESIAN_POINT ( 'NONE',  ( 1.394999999999999574, -19.67366047555544739, 20.02152543075338897 ) ) ;
#1009 = FACE_OUTER_BOUND ( 'NONE', #10518, .T. ) ;
#1010 = CARTESIAN_POINT ( 'NONE',  ( 2.508169608347903257, -5.259531939870091932, -15.25429862889487076 ) ) ;
#1011 = CYLINDRICAL_SURFACE ( 'NONE', #187, 13.19999999999999929 ) ;
#1012 = CARTESIAN_POINT ( 'NONE',  ( 0.000000000000000000, 0.000000000000000000, -7.000000000000007994 ) ) ;
#1013 = VERTEX_POINT ( 'NONE', #13943 ) ;
#1014 = DIRECTION ( 'NONE',  ( -1.445602896647338917E-16, 1.000000000000000000, -0.000000000000000000 ) ) ;
#1015 = DIRECTION ( 'NONE',  ( 0.000000000000000000, -1.374038396813314756E-15, -1.000000000000000000 ) ) ;
#1016 = ADVANCED_FACE ( 'NONE', ( #8104 ), #8886, .T. ) ;
#1017 = SHAPE_REPRESENTATION ( 'plate 1', ( #1376 ), #2887 ) ;
#1018 = CARTESIAN_POINT ( 'NONE',  ( 2.765633920072238627, 5.391175441198956086, -24.15498966839956907 ) ) ;
#1019 = EDGE_CURVE ( 'NONE', #12415, #5464, #10648, .T. ) ;
#1020 = EDGE_CURVE ( 'NONE', #4343, #12388, #6600, .T. ) ;
#1021 = B_SPLINE_CURVE_WITH_KNOTS ( 'NONE', 3,
 ( #9744, #3909, #1597, #13271, #2751, #7443 ),
 .UNSPECIFIED., .F., .F.,
 ( 4, 2, 4 ),
 ( 0.0009182716802120147702, 0.002354250892314196063, 0.003790230104416377789 ),
 .UNSPECIFIED. ) ;
#1022 = ORIENTED_EDGE ( 'NONE', *, *, #1967, .T. ) ;
#1023 = CARTESIAN_POINT ( 'NONE',  ( 10.00000000000000178, -1.390791565672601315, -130.1575142076926852 ) ) ;
#1024 = PLANE ( 'NONE',  #2586 ) ;
#1025 = ORIENTED_EDGE ( 'NONE', *, *, #12744, .F. ) ;
#1026 = ORIENTED_EDGE ( 'NONE', *, *, #9932, .T. ) ;
#1027 = DIRECTION ( 'NONE',  ( 0.000000000000000000, 0.000000000000000000, 1.000000000000000000 ) ) ;
#1028 = B_SPLINE_CURVE_WITH_KNOTS ( 'NONE', 3,
 ( #7224, #7076, #7152, #5858, #10543, #6075 ),
 .UNSPECIFIED., .F., .F.,
 ( 4, 2, 4 ),
 ( 0.0009182716802119580664, 0.002354250892314169608, 0.003790230104416381259 ),
 .UNSPECIFIED. ) ;
#1029 = ORIENTED_EDGE ( 'NONE', *, *, #3499, .T. ) ;
#1030 = AXIS2_PLACEMENT_3D ( 'NONE', #14428, #2890, #1737 ) ;
#1031 = FACE_OUTER_BOUND ( 'NONE', #13641, .T. ) ;
#1032 = CARTESIAN_POINT ( 'NONE',  ( 0.000000000000000000, -8.624777288397730501, -11.04103753892280615 ) ) ;
#1033 = LINE ( 'NONE', #10334, #13131 ) ;
#1034 = CARTESIAN_POINT ( 'NONE',  ( 1.955868201400819517, -16.87476974924773288, 4.976599981640283943 ) ) ;
#1035 = ORIENTED_EDGE ( 'NONE', *, *, #4321, .T. ) ;
#1036 = LINE ( 'NONE', #6952, #3612 ) ;
#1037 = DIRECTION ( 'NONE',  ( -1.000000000000000000, 0.000000000000000000, 0.000000000000000000 ) ) ;
#1038 = ORIENTED_EDGE ( 'NONE', *, *, #13176, .T. ) ;
#1039 = AXIS2_PLACEMENT_3D ( 'NONE', #11466, #13547, #2022 ) ;
#1040 = AXIS2_PLACEMENT_3D ( 'NONE', #959, #9113, #11262 ) ;
#1041 = ORIENTED_EDGE ( 'NONE', *, *, #264, .T. ) ;
#1042 = CARTESIAN_POINT ( 'NONE',  ( 1.039999999999996483, -12.96210679857803783, 24.89775460606827551 ) ) ;
#1043 = CARTESIAN_POINT ( 'NONE',  ( 59.43001430450886602, 34.23215029930534570, -2.000000000000000000 ) ) ;
#1044 = EDGE_CURVE ( 'NONE', #5009, #9526, #161, .T. ) ;
#1045 = CYLINDRICAL_SURFACE ( 'NONE', #11953, 0.5999999999999998668 ) ;
#1046 = CARTESIAN_POINT ( 'NONE',  ( 0.02436607992776585255, -5.391175441198789109, 24.15498966839961170 ) ) ;
#1047 = DIRECTION ( 'NONE',  ( 1.000000000000000000, 0.000000000000000000, 0.000000000000000000 ) ) ;
#1048 = CARTESIAN_POINT ( 'NONE',  ( 2.765633920072239516, -24.15498966839958683, -5.391175441198872598 ) ) ;
#1049 = ORIENTED_EDGE ( 'NONE', *, *, #13787, .F. ) ;
#1051 = AXIS2_PLACEMENT_3D ( 'NONE', #4024, #8698, #9937 ) ;
#1050 = FACE_OUTER_BOUND ( 'NONE', #6316, .T. ) ;
#1052 = CARTESIAN_POINT ( 'NONE',  ( 2.789999999999999147, 14.55412442567645215, -19.64056340710859772 ) ) ;
#1053 = FACE_OUTER_BOUND ( 'NONE', #6273, .T. ) ;
#1054 = DIRECTION ( 'NONE',  ( -1.000000000000000000, -0.000000000000000000, 0.000000000000000000 ) ) ;
#1055 = VERTEX_POINT ( 'NONE', #4726 ) ;
#1056 = B_SPLINE_CURVE_WITH_KNOTS ( 'NONE', 3,
 ( #14995, #4461, #9141, #9299 ),
 .UNSPECIFIED., .F., .F.,
 ( 4, 4 ),
 ( 2.324263106244727961E-07, 0.0006888201370294844746 ),
 .UNSPECIFIED. ) ;
#1057 = EDGE_CURVE ( 'NONE', #10796, #3392, #11919, .T. ) ;
#1058 = LINE ( 'NONE', #4893, #2111 ) ;
#1059 = DIRECTION ( 'NONE',  ( -0.000000000000000000, -0.000000000000000000, 1.000000000000000000 ) ) ;
#1060 = EDGE_LOOP ( 'NONE', ( #3025, #4253, #9240, #3645 ) ) ;
#1061 = VERTEX_POINT ( 'NONE', #2412 ) ;
#1062 = CARTESIAN_POINT ( 'NONE',  ( 2.789999999999999147, -25.59481291497571220, -1.787276233276378314E-13 ) ) ;
#1063 = DIRECTION ( 'NONE',  ( -1.000000000000000000, -0.000000000000000000, -0.000000000000000000 ) ) ;
#1064 = ORIENTED_EDGE ( 'NONE', *, *, #629, .F. ) ;
#1065 = CARTESIAN_POINT ( 'NONE',  ( 2.789999999999999147, 7.909232158575156824, -24.34211360614291664 ) ) ;
#1066 = CARTESIAN_POINT ( 'NONE',  ( -10.00000000000000000, 0.000000000000000000, 0.000000000000000000 ) ) ;
#1067 = DIRECTION ( 'NONE',  ( 0.000000000000000000, 0.000000000000000000, 1.000000000000000000 ) ) ;
#1068 = DIRECTION ( 'NONE',  ( 0.000000000000000000, 0.000000000000000000, 1.000000000000000000 ) ) ;
#1069 = DIRECTION ( 'NONE',  ( -0.7757024858236036824, 0.6310987668242443727, 2.080818337223229247E-17 ) ) ;
#1070 = EDGE_CURVE ( 'NONE', #13441, #8611, #4771, .T. ) ;
#1071 = VERTEX_POINT ( 'NONE', #1409 ) ;
#1072 = CARTESIAN_POINT ( 'NONE',  ( 2.789999999999999147, -24.63872515616080960, -2.336989772644527008 ) ) ;
#1073 = DIRECTION ( 'NONE',  ( -1.000000000000000000, 0.000000000000000000, -0.000000000000000000 ) ) ;
#1074 = ADVANCED_FACE ( 'NONE', ( #9706 ), #13240, .F. ) ;
#1075 = EDGE_LOOP ( 'NONE', ( #12142, #6161 ) ) ;
#1076 = FILL_AREA_STYLE ('',( #8295 ) ) ;
#1077 = ORIENTED_EDGE ( 'NONE', *, *, #7513, .F. ) ;
#1078 = ORIENTED_EDGE ( 'NONE', *, *, #5790, .F. ) ;
#1079 = EDGE_LOOP ( 'NONE', ( #2513, #15023, #6182, #877 ) ) ;
#1080 = DIRECTION ( 'NONE',  ( -5.339417856040273846E-17, -1.063174570779084847E-17, 1.000000000000000000 ) ) ;
#1081 = FACE_OUTER_BOUND ( 'NONE', #1333, .T. ) ;
#1082 = CLOSED_SHELL ( 'NONE', ( #13807, #8527, #4660, #7191, #6991, #11941, #10621, #225, #1968, #4967, #10970, #9272, #726, #4847, #5728, #6700, #3383, #3396, #7586, #1751, #12998, #2428, #2056, #9460, #10685, #12723, #3621, #9453, #10423, #11678, #5875, #5344, #7238, #9097, #1004, #1780, #1937, #11299, #9087, #13708, #5635, #2775, #13518, #5185, #236, #6070, #463, #12791, #1074, #11354, #10231, #10765, #4415, #3764, #5637, #14346, #11847, #4400, #4712, #15088, #3270, #822, #8033, #10158, #4186, #66, #12267, #2450, #11769, #1118, #7211, #9365, #3656, #9856, #539, #13279, #6798, #5189, #10942, #5043, #10869, #6169, #14947 ) ) ;
#1083 = CARTESIAN_POINT ( 'NONE',  ( 0.04999670013151481102, -9.490919315500054410, -11.55877992729675263 ) ) ;
#1084 = DIRECTION ( 'NONE',  ( 0.000000000000000000, 0.000000000000000000, 1.000000000000000000 ) ) ;
#1085 = AXIS2_PLACEMENT_3D ( 'NONE', #14018, #3483, #4499 ) ;
#1086 = CARTESIAN_POINT ( 'NONE',  ( 1.039999999999997593, -4.458161950358380032, -17.39253030560846369 ) ) ;
#1087 = EDGE_LOOP ( 'NONE', ( #8142, #8059, #9530, #56 ) ) ;
#1088 = AXIS2_PLACEMENT_3D ( 'NONE', #3058, #5452, #751 ) ;
#1089 = CARTESIAN_POINT ( 'NONE',  ( 1.249999999999997558, 0.000000000000000000, 0.000000000000000000 ) ) ;
#1090 = CARTESIAN_POINT ( 'NONE',  ( 33.82574562093736859, -6.697933970950280091, 7.000000000000000000 ) ) ;
#1091 = VECTOR ( 'NONE', #6616, 1000.000000000000000 ) ;
#1092 = AXIS2_PLACEMENT_3D ( 'NONE', #13318, #5127, #5044 ) ;
#1093 = EDGE_CURVE ( 'NONE', #6683, #14792, #3780, .T. ) ;
#1094 = ORIENTED_EDGE ( 'NONE', *, *, #10759, .F. ) ;
#1095 = FACE_BOUND ( 'NONE', #9322, .T. ) ;
#1096 = LINE ( 'NONE', #15093, #3554 ) ;
#1097 = ORIENTED_EDGE ( 'NONE', *, *, #1791, .T. ) ;
#1098 = ORIENTED_EDGE ( 'NONE', *, *, #9625, .T. ) ;
#1099 = CARTESIAN_POINT ( 'NONE',  ( -14.40394475573011235, 8.328953704812679362E-15, 16.99999999999999645 ) ) ;
#1100 = AXIS2_PLACEMENT_3D ( 'NONE', #502, #5221, #6207 ) ;
#1101 = EDGE_CURVE ( 'NONE', #4663, #6635, #14169, .T. ) ;
#1102 = AXIS2_PLACEMENT_3D ( 'NONE', #2865, #3021, #11084 ) ;
#1103 = ADVANCED_FACE ( 'NONE', ( #9624 ), #2487, .F. ) ;
#1104 = VERTEX_POINT ( 'NONE', #14401 ) ;
#1105 = VECTOR ( 'NONE', #3625, 1000.000000000000000 ) ;
#1106 = CARTESIAN_POINT ( 'NONE',  ( 2.246812850058911071, 16.16568790143448453, -5.154374911958746530 ) ) ;
#1107 = CYLINDRICAL_SURFACE ( 'NONE', #11751, 4.000000000000000000 ) ;
#1108 = CARTESIAN_POINT ( 'NONE',  ( 1.039999999999996261, 12.83329210556831512, 12.55714665599991697 ) ) ;
#1109 = LINE ( 'NONE', #4729, #8437 ) ;
#1110 = VERTEX_POINT ( 'NONE', #14319 ) ;
#1111 = DIRECTION ( 'NONE',  ( 1.576560579138138762E-17, -1.359337748750801608E-17, 1.000000000000000000 ) ) ;
#1112 = CARTESIAN_POINT ( 'NONE',  ( 1.394999999999999574, -25.12109765559644714, -12.52377138324250616 ) ) ;
#1113 = ORIENTED_EDGE ( 'NONE', *, *, #10018, .F. ) ;
#1114 = CIRCLE ( 'NONE', #5058, 2.999999999999975131 ) ;
#1115 = AXIS2_PLACEMENT_3D ( 'NONE', #3624, #4719, #10846 ) ;
#1116 = AXIS2_PLACEMENT_3D ( 'NONE', #3202, #7653, #7884 ) ;
#1117 = ORIENTED_EDGE ( 'NONE', *, *, #12181, .F. ) ;
#1118 = ADVANCED_FACE ( 'NONE', ( #8466 ), #7171, .T. ) ;
#1119 = CARTESIAN_POINT ( 'NONE',  ( 0.000000000000000000, 8.624777288397959651, -11.04103753892262674 ) ) ;
#1120 = DIRECTION ( 'NONE',  ( 1.000000000000000000, -0.000000000000000000, 0.000000000000000000 ) ) ;
#1121 = EDGE_CURVE ( 'NONE', #2246, #12653, #6172, .T. ) ;
#1122 = DIRECTION ( 'NONE',  ( 0.02857142857142857401, 0.9995917534020515305, -0.000000000000000000 ) ) ;
#1123 = DIRECTION ( 'NONE',  ( 0.000000000000000000, 0.000000000000000000, 1.000000000000000000 ) ) ;
#1124 = FACE_OUTER_BOUND ( 'NONE', #2162, .T. ) ;
#1125 = PRODUCT_DEFINITION_SHAPE ( 'NONE', 'NONE',  #15229 ) ;
#1126 = EDGE_CURVE ( 'NONE', #1971, #10848, #12626, .T. ) ;
#1127 = CARTESIAN_POINT ( 'NONE',  ( 80.00000000000000000, 0.000000000000000000, 4.500000000000000888 ) ) ;
#1128 = AXIS2_PLACEMENT_3D ( 'NONE', #1483, #12308, #10849 ) ;
#1129 = ORIENTED_EDGE ( 'NONE', *, *, #3944, .F. ) ;
#1130 = PLANE ( 'NONE',  #5867 ) ;
#1131 = LINE ( 'NONE', #9501, #6687 ) ;
#1132 = CARTESIAN_POINT ( 'NONE',  ( 1.749999999999999778, 0.000000000000000000, 0.000000000000000000 ) ) ;
#1133 = FACE_BOUND ( 'NONE', #9789, .T. ) ;
#1134 = EDGE_CURVE ( 'NONE', #3521, #6501, #14102, .T. ) ;
#1135 = EDGE_LOOP ( 'NONE', ( #6017, #411, #13009, #12237, #2229, #1097, #5536, #3727 ) ) ;
#1136 = VERTEX_POINT ( 'NONE', #10785 ) ;
#1137 = CIRCLE ( 'NONE', #7021, 3.000000000000002665 ) ;
#1138 = CARTESIAN_POINT ( 'NONE',  ( 2.789999999999999147, -7.739906618939614624, -10.88091150984234545 ) ) ;
#1139 = ORIENTED_EDGE ( 'NONE', *, *, #2318, .T. ) ;
#1140 = CARTESIAN_POINT ( 'NONE',  ( 0.008751532933531189218, -13.40591150985895297, -5.214906618939850524 ) ) ;
#1141 = VECTOR ( 'NONE', #594, 1000.000000000000000 ) ;
#1142 = CARTESIAN_POINT ( 'NONE',  ( 1.666666666666673624, 0.000000000000000000, -130.1575142076926852 ) ) ;
#1143 = STYLED_ITEM ( 'NONE', ( #464 ), #476 ) ;
#1144 = CARTESIAN_POINT ( 'NONE',  ( 1.039999999999997593, 0.000000000000000000, 0.000000000000000000 ) ) ;
#1145 = CARTESIAN_POINT ( 'NONE',  ( 0.000000000000000000, 0.4273491293402468805, -0.8000000000000000444 ) ) ;
#1146 = DIRECTION ( 'NONE',  ( 1.000000000000000000, 0.000000000000000000, 0.000000000000000000 ) ) ;
#1147 = DIRECTION ( 'NONE',  ( 1.000000000000000000, 0.000000000000000000, 0.000000000000000000 ) ) ;
#1148 = CARTESIAN_POINT ( 'NONE',  ( 2.789999999999999147, 0.000000000000000000, 0.000000000000000000 ) ) ;
#1149 = VERTEX_POINT ( 'NONE', #237 ) ;
#1150 = AXIS2_PLACEMENT_3D ( 'NONE', #1436, #14196, #4910 ) ;
#1151 = AXIS2_PLACEMENT_3D ( 'NONE', #529, #13228, #10915 ) ;
#1152 = CARTESIAN_POINT ( 'NONE',  ( 0.7795480763126773072, 11.98750039041511961, -12.70439593876648132 ) ) ;
#1153 = ORIENTED_EDGE ( 'NONE', *, *, #7233, .F. ) ;
#1154 = PRESENTATION_LAYER_ASSIGNMENT (  '', '', ( #7781 ) ) ;
#1155 = AXIS2_PLACEMENT_3D ( 'NONE', #2651, #6177, #5122 ) ;
#1156 = EDGE_CURVE ( 'NONE', #516, #5499, #14365, .T. ) ;
#1157 = CIRCLE ( 'NONE', #5838, 4.000000000000000888 ) ;
#1158 = VERTEX_POINT ( 'NONE', #12922 ) ;
#1159 = ORIENTED_EDGE ( 'NONE', *, *, #1020, .T. ) ;
#1160 = ORIENTED_EDGE ( 'NONE', *, *, #7864, .F. ) ;
#1161 = PLANE ( 'NONE',  #7041 ) ;
#1162 = CARTESIAN_POINT ( 'NONE',  ( 1.749999999999998002, -27.68468304288262516, 4.633866840648810381 ) ) ;
#1163 =( GEOMETRIC_REPRESENTATION_CONTEXT ( 3 ) GLOBAL_UNCERTAINTY_ASSIGNED_CONTEXT ( ( #8003 ) ) GLOBAL_UNIT_ASSIGNED_CONTEXT ( ( #961, #13644, #10039 ) ) REPRESENTATION_CONTEXT ( 'NONE', 'WORKASPACE' ) );
#1164 = CARTESIAN_POINT ( 'NONE',  ( 0.007327513813774171221, 5.204526028255878067, -13.44898112152233338 ) ) ;
#1165 = CARTESIAN_POINT ( 'NONE',  ( 1.749999999999998002, -24.89775460606842117, 12.96210679857777137 ) ) ;
#1166 = CIRCLE ( 'NONE', #11222, 10.00000000000000000 ) ;
#1167 = CARTESIAN_POINT ( 'NONE',  ( 1.000000000000000000, -4.808326913195983821, 0.000000000000000000 ) ) ;
#1168 = CIRCLE ( 'NONE', #14164, 9.999999999999994671 ) ;
#1169 = ORIENTED_EDGE ( 'NONE', *, *, #8068, .F. ) ;
#1170=STYLED_ITEM('',(#15265),#9040);
#1171 = LINE ( 'NONE', #10842, #10236 ) ;
#1172 = VECTOR ( 'NONE', #15011, 1000.000000000000000 ) ;
#1173 = ORIENTED_EDGE ( 'NONE', *, *, #10150, .T. ) ;
#1174 = CARTESIAN_POINT ( 'NONE',  ( 8.961831343790189308, 9.104486995144789319, 3.000000000000002665 ) ) ;
#1175 = CARTESIAN_POINT ( 'NONE',  ( -5.999999999999999112, 0.000000000000000000, 1.395000000000000462 ) ) ;
#1176 = ORIENTED_EDGE ( 'NONE', *, *, #2059, .T. ) ;
#1177 = ORIENTED_EDGE ( 'NONE', *, *, #2258, .T. ) ;
#1178 = TOROIDAL_SURFACE ( 'NONE', #3629, 5.000000000000000000, 0.5999999999999999778 ) ;
#1179 = ADVANCED_FACE ( 'NONE', ( #3555 ), #5032, .F. ) ;
#1180 = DIRECTION ( 'NONE',  ( 0.000000000000000000, 0.000000000000000000, 1.000000000000000000 ) ) ;
#1181 = VERTEX_POINT ( 'NONE', #1182 ) ;
#1182 = CARTESIAN_POINT ( 'NONE',  ( 76.00000000000000000, 4.898587196589422689E-16, 4.500000000000003553 ) ) ;
#1183 = EDGE_CURVE ( 'NONE', #12755, #132, #7011, .T. ) ;
#1184 = AXIS2_PLACEMENT_3D ( 'NONE', #13289, #8751, #6304 ) ;
#1185 = CARTESIAN_POINT ( 'NONE',  ( 83.50748565343083385, 13.38500995229612478, 2.999999999999999112 ) ) ;
#1186 = DIRECTION ( 'NONE',  ( -1.000000000000000000, -0.000000000000000000, -0.000000000000000000 ) ) ;
#1187 = CARTESIAN_POINT ( 'NONE',  ( 2.429628795537856156, -15.53862542373106237, 5.230001598524554929 ) ) ;
#1188 = AXIS2_PLACEMENT_3D ( 'NONE', #7647, #14417, #6413 ) ;
#1189 = ORIENTED_EDGE ( 'NONE', *, *, #8120, .T. ) ;
#1190 = TOROIDAL_SURFACE ( 'NONE', #14951, 24.12539914357697768, 8.000000000000000000 ) ;
#1191 = CARTESIAN_POINT ( 'NONE',  ( 111.6227766016837961, 7.610970684806392799E-15, -130.1575142076926852 ) ) ;
#1192 = CARTESIAN_POINT ( 'NONE',  ( 101.4858053992934401, 0.9022481406819604643, -2.000000000000000888 ) ) ;
#1193 = ORIENTED_EDGE ( 'NONE', *, *, #15025, .F. ) ;
#1194 = EDGE_CURVE ( 'NONE', #4401, #3473, #10561, .T. ) ;
#1195 = ADVANCED_FACE ( 'NONE', ( #13619 ), #7733, .T. ) ;
#1196 = EDGE_LOOP ( 'NONE', ( #110, #1509, #11563, #8866 ) ) ;
#1197 = CARTESIAN_POINT ( 'NONE',  ( 0.2076373605413187606, -5.278564329441106651, 14.94126095370959462 ) ) ;
#1198 = CYLINDRICAL_SURFACE ( 'NONE', #442, 2.524999999999995914 ) ;
#1199 = DIRECTION ( 'NONE',  ( -0.000000000000000000, -0.000000000000000000, 1.000000000000000000 ) ) ;
#1200 = CYLINDRICAL_SURFACE ( 'NONE', #10445, 5.000000000000000888 ) ;
#1201 = CIRCLE ( 'NONE', #2400, 0.5999999999999999778 ) ;
#1203 = DIRECTION ( 'NONE',  ( -1.000000000000000000, -0.000000000000000000, -0.000000000000000000 ) ) ;
#1202 = VECTOR ( 'NONE', #1786, 1000.000000000000000 ) ;
#1204 = CARTESIAN_POINT ( 'NONE',  ( 2.789999999999999147, 13.40591150984226587, 7.739906618939754956 ) ) ;
#1205 = ORIENTED_EDGE ( 'NONE', *, *, #12615, .F. ) ;
#1206 = DIRECTION ( 'NONE',  ( 0.000000000000000000, 0.000000000000000000, -1.000000000000000000 ) ) ;
#1207 = CARTESIAN_POINT ( 'NONE',  ( 0.07181525480391370841, -12.74223776959215826, 21.92234060054341427 ) ) ;
#1208 = CARTESIAN_POINT ( 'NONE',  ( 88.84370878116858705, 10.64188714589527507, 7.000000000000000000 ) ) ;
#1209 = CARTESIAN_POINT ( 'NONE',  ( 2.718184749312773540, -2.576941577947583273, 25.22524549359949120 ) ) ;
#1210 = EDGE_CURVE ( 'NONE', #13239, #949, #1314, .T. ) ;
#1211 = EDGE_LOOP ( 'NONE', ( #2408, #10707 ) ) ;
#1212 = AXIS2_PLACEMENT_3D ( 'NONE', #1541, #6456, #606 ) ;
#1213 = ORIENTED_EDGE ( 'NONE', *, *, #1383, .T. ) ;
#1214 = EDGE_CURVE ( 'NONE', #2185, #99, #4050, .T. ) ;
#1215 = CARTESIAN_POINT ( 'NONE',  ( 2.765633920072236851, -22.71065055754445439, -9.836394144775947979 ) ) ;
#1216 = ORIENTED_EDGE ( 'NONE', *, *, #6764, .F. ) ;
#1217 = CARTESIAN_POINT ( 'NONE',  ( 2.789999999999999147, -7.772527002114597572, 23.17675759782038369 ) ) ;
#1218 = DIRECTION ( 'NONE',  ( 0.000000000000000000, 0.000000000000000000, -1.000000000000000000 ) ) ;
#1219 = DIRECTION ( 'NONE',  ( 0.000000000000000000, 0.000000000000000000, -1.000000000000000000 ) ) ;
#1220 = CARTESIAN_POINT ( 'NONE',  ( 0.008751532932800723183, 13.40591150984233870, -5.214906618939568084 ) ) ;
#1221 = B_SPLINE_CURVE_WITH_KNOTS ( 'NONE', 3,
 ( #5472, #4235, #9145, #3233, #7918, #8909 ),
 .UNSPECIFIED., .F., .F.,
 ( 4, 2, 4 ),
 ( 4.462636882273700183E-07, 0.001879885203074810199, 0.003759324142461393028 ),
 .UNSPECIFIED. ) ;
#1222 = CARTESIAN_POINT ( 'NONE',  ( 0.02531912748464718033, -14.46287784598619020, 2.311161484776505404 ) ) ;
#1223 = EDGE_CURVE ( 'NONE', #8917, #4042, #1637, .T. ) ;
#1224 = DIRECTION ( 'NONE',  ( -1.000000000000000000, -0.000000000000000000, -0.000000000000000000 ) ) ;
#1225 = DIRECTION ( 'NONE',  ( 0.2314933715733012709, -0.9728364810787194505, 0.000000000000000000 ) ) ;
#1226 = ADVANCED_BREP_SHAPE_REPRESENTATION ( '', ( #8904, #1376 ), #11929 ) ;
#1227 = CIRCLE ( 'NONE', #1977, 4.000000000000000000 ) ;
#1228 = ORIENTED_EDGE ( 'NONE', *, *, #113, .T. ) ;
#1229 = DIRECTION ( 'NONE',  ( 0.000000000000000000, 0.000000000000000000, 1.000000000000000000 ) ) ;
#1230 = LINE ( 'NONE', #5986, #13850 ) ;
#1231 = ORIENTED_EDGE ( 'NONE', *, *, #5249, .F. ) ;
#1232 = ORIENTED_EDGE ( 'NONE', *, *, #3988, .F. ) ;
#1233 = EDGE_LOOP ( 'NONE', ( #2848, #13553 ) ) ;
#1234 = VERTEX_POINT ( 'NONE', #9858 ) ;
#1235 = VECTOR ( 'NONE', #28, 1000.000000000000000 ) ;
#1236 = CYLINDRICAL_SURFACE ( 'NONE', #401, 31.62277660168379256 ) ;
#1237 = DIRECTION ( 'NONE',  ( 0.000000000000000000, 0.000000000000000000, 1.000000000000000000 ) ) ;
#1238 = CYLINDRICAL_SURFACE ( 'NONE', #11480, 9.999999999999994671 ) ;
#1239 = DIRECTION ( 'NONE',  ( 0.000000000000000000, 0.000000000000000000, 1.000000000000000000 ) ) ;
#1240 = FACE_OUTER_BOUND ( 'NONE', #4768, .T. ) ;
#1241 = ORIENTED_EDGE ( 'NONE', *, *, #12909, .F. ) ;
#1242 = B_SPLINE_CURVE_WITH_KNOTS ( 'NONE', 3,
 ( #4683, #11726, #11866, #3506, #1209, #9581 ),
 .UNSPECIFIED., .F., .F.,
 ( 4, 2, 4 ),
 ( 4.462636732217463004E-07, 0.001879885066975006029, 0.003759323870276790047 ),
 .UNSPECIFIED. ) ;
#1243 = DIRECTION ( 'NONE',  ( -0.000000000000000000, -0.000000000000000000, -1.000000000000000000 ) ) ;
#1244 = ORIENTED_EDGE ( 'NONE', *, *, #9119, .F. ) ;
#1245 = DIRECTION ( 'NONE',  ( -0.9863939238321437486, -0.1643989873053572359, 0.000000000000000000 ) ) ;
#1246 = FACE_OUTER_BOUND ( 'NONE', #3129, .T. ) ;
#1247 = EDGE_CURVE ( 'NONE', #7097, #4081, #548, .T. ) ;
#1248 = ORIENTED_EDGE ( 'NONE', *, *, #12434, .T. ) ;
#1249 = VERTEX_POINT ( 'NONE', #12389 ) ;
#1250 = CARTESIAN_POINT ( 'NONE',  ( 10.40394475573011945, -10.79473832354794460, 6.000000000000000000 ) ) ;
#1251 = ORIENTED_EDGE ( 'NONE', *, *, #5443, .T. ) ;
#1252 = DIRECTION ( 'NONE',  ( 0.000000000000000000, 0.000000000000000000, 1.000000000000000000 ) ) ;
#1253 = LINE ( 'NONE', #10562, #4367 ) ;
#1254 = EDGE_CURVE ( 'NONE', #10971, #5354, #13309, .T. ) ;
#1255 = CARTESIAN_POINT ( 'NONE',  ( 1.749999999999998002, -4.147968289691484678, 27.76164181293050603 ) ) ;
#1256 = CYLINDRICAL_SURFACE ( 'NONE', #13602, 4.000000000000000000 ) ;
#1257 = ORIENTED_EDGE ( 'NONE', *, *, #3095, .T. ) ;
#1258 = DIRECTION ( 'NONE',  ( 0.000000000000000000, 0.000000000000000000, -1.000000000000000000 ) ) ;
#1259 = EDGE_CURVE ( 'NONE', #9849, #13077, #7974, .T. ) ;
#1260 = CARTESIAN_POINT ( 'NONE',  ( 2.789999999999999147, -12.98979500319697955, 5.249430348645709010 ) ) ;
#1261 = ORIENTED_EDGE ( 'NONE', *, *, #10893, .T. ) ;
#1262 = ORIENTED_EDGE ( 'NONE', *, *, #9472, .T. ) ;
#1263 = LINE ( 'NONE', #4589, #12939 ) ;
#1264 = CARTESIAN_POINT ( 'NONE',  ( 0.000000000000000000, -1.948757464274081030, -13.87420763704363580 ) ) ;
#1265 = DIRECTION ( 'NONE',  ( 0.000000000000000000, 0.000000000000000000, 1.000000000000000000 ) ) ;
#1266 = DIRECTION ( 'NONE',  ( 0.000000000000000000, -6.870191984066573782E-16, -1.000000000000000000 ) ) ;
#1267 = DIRECTION ( 'NONE',  ( 0.000000000000000000, 3.435095992033281961E-15, -1.000000000000000000 ) ) ;
#1268 = FACE_OUTER_BOUND ( 'NONE', #5575, .T. ) ;
#1269 = EDGE_CURVE ( 'NONE', #7725, #1234, #4254, .T. ) ;
#1270 = ORIENTED_EDGE ( 'NONE', *, *, #12382, .F. ) ;
#1271 = CARTESIAN_POINT ( 'NONE',  ( -14.40394475573011945, -10.79473832354794460, 0.7999999999999960476 ) ) ;
#1272 = CARTESIAN_POINT ( 'NONE',  ( 0.000000000000000000, 0.000000000000000000, 0.000000000000000000 ) ) ;
#1273 = CARTESIAN_POINT ( 'NONE',  ( -9.403944755730117677, -13.79473832354794993, 16.99999999999999645 ) ) ;
#1274 = CYLINDRICAL_SURFACE ( 'NONE', #4844, 8.399999999999998579 ) ;
#1275 = VERTEX_POINT ( 'NONE', #1868 ) ;
#1276 = ORIENTED_EDGE ( 'NONE', *, *, #7099, .T. ) ;
#1277 = EDGE_CURVE ( 'NONE', #799, #3527, #1714, .T. ) ;
#1278 = VERTEX_POINT ( 'NONE', #7480 ) ;
#1279 = FACE_OUTER_BOUND ( 'NONE', #7657, .T. ) ;
#1280 = LINE ( 'NONE', #8132, #6582 ) ;
#1281 = CARTESIAN_POINT ( 'NONE',  ( 101.6227766016837819, -9.999999999999994671, 7.000000000000000000 ) ) ;
#1282 = CARTESIAN_POINT ( 'NONE',  ( 2.782650494170373356, 13.44926448535263042, 5.204557061642334226 ) ) ;
#1283 = DIRECTION ( 'NONE',  ( 0.000000000000000000, 0.000000000000000000, -1.000000000000000000 ) ) ;
#1284 = DIRECTION ( 'NONE',  ( -1.000000000000000000, -0.000000000000000000, -0.000000000000000000 ) ) ;
#1285 = EDGE_CURVE ( 'NONE', #14210, #12453, #13387, .T. ) ;
#1286 = VECTOR ( 'NONE', #5600, 1000.000000000000000 ) ;
#1287 = ORIENTED_EDGE ( 'NONE', *, *, #1044, .T. ) ;
#1288 = DIRECTION ( 'NONE',  ( 0.000000000000000000, -1.000000000000000000, 0.000000000000000000 ) ) ;
#1289 = DIRECTION ( 'NONE',  ( -1.000000000000000000, 0.000000000000000000, -0.000000000000000000 ) ) ;
#1290 = EDGE_CURVE ( 'NONE', #12512, #11686, #5017, .T. ) ;
#1291 = ADVANCED_FACE ( 'NONE', ( #1554 ), #4791, .T. ) ;
#1292 = ORIENTED_EDGE ( 'NONE', *, *, #13403, .F. ) ;
#1293 = PLANE ( 'NONE',  #8047 ) ;
#1294 = CARTESIAN_POINT ( 'NONE',  ( 0.02436607992776064838, 18.55949924794892780, 16.37294372382865504 ) ) ;
#1295 = CARTESIAN_POINT ( 'NONE',  ( 0.9661342547375842971, -24.74813374239834474, 12.96725027898183669 ) ) ;
#1296 = VERTEX_POINT ( 'NONE', #394 ) ;
#1297 = ORIENTED_EDGE ( 'NONE', *, *, #12952, .T. ) ;
#1298 = ORIENTED_EDGE ( 'NONE', *, *, #14707, .F. ) ;
#1299 = ORIENTED_EDGE ( 'NONE', *, *, #10463, .T. ) ;
#1300 = FACE_OUTER_BOUND ( 'NONE', #5332, .T. ) ;
#1301 = DIRECTION ( 'NONE',  ( -0.9863939238321436376, -0.1643989873053573192, 0.000000000000000000 ) ) ;
#1302 = DIRECTION ( 'NONE',  ( -0.9863939238321437486, -0.1643989873053574857, 0.000000000000000000 ) ) ;
#1303 = CARTESIAN_POINT ( 'NONE',  ( 1.749999999999999778, -12.55714665599977842, -12.83329210556845190 ) ) ;
#1304 = ADVANCED_FACE ( 'NONE', ( #9929 ), #6556, .T. ) ;
#1305 = ADVANCED_FACE ( 'NONE', ( #13545 ), #713, .T. ) ;
#1306 = CARTESIAN_POINT ( 'NONE',  ( 2.764680872515351773, 11.36963888406687317, 9.232963481057801403 ) ) ;
#1307 = EDGE_CURVE ( 'NONE', #316, #446, #12152, .T. ) ;
#1308 = ORIENTED_EDGE ( 'NONE', *, *, #12340, .F. ) ;
#1309 = DIRECTION ( 'NONE',  ( 0.000000000000000000, 0.000000000000000000, 1.000000000000000000 ) ) ;
#1310 = EDGE_CURVE ( 'NONE', #6398, #6064, #7237, .T. ) ;
#1311 = PRODUCT_DEFINITION_FORMATION_WITH_SPECIFIED_SOURCE ( 'ANY', '', #13509, .NOT_KNOWN. ) ;
#1312 = ORIENTED_EDGE ( 'NONE', *, *, #4480, .F. ) ;
#1313 = DIRECTION ( 'NONE',  ( 0.000000000000000000, 0.000000000000000000, 1.000000000000000000 ) ) ;
#1314 = B_SPLINE_CURVE_WITH_KNOTS ( 'NONE', 3,
 ( #7561, #2785, #3102, #7705, #8623, #5420 ),
 .UNSPECIFIED., .F., .F.,
 ( 4, 2, 4 ),
 ( 4.462636882221863355E-07, 0.001879885203074805429, 0.003759324142461388692 ),
 .UNSPECIFIED. ) ;
#1315 = B_SPLINE_CURVE_WITH_KNOTS ( 'NONE', 3,
 ( #10884, #14355, #9966, #14666, #3817, #7661 ),
 .UNSPECIFIED., .F., .F.,
 ( 4, 2, 4 ),
 ( 2.586195665735896780E-07, 0.001878649493629692057, 0.003757040367692810780 ),
 .UNSPECIFIED. ) ;
#1316 = VERTEX_POINT ( 'NONE', #12473 ) ;
#1317 = ORIENTED_EDGE ( 'NONE', *, *, #8230, .T. ) ;
#1318 = TOROIDAL_SURFACE ( 'NONE', #336, 24.12539914357697413, 8.000000000000000000 ) ;
#1319 = CARTESIAN_POINT ( 'NONE',  ( 19.20634328910001543, -26.21503864878155099, 4.000000000000000000 ) ) ;
#1320 = ORIENTED_EDGE ( 'NONE', *, *, #13609, .F. ) ;
#1321 = DIRECTION ( 'NONE',  ( -1.000000000000000000, -0.000000000000000000, -0.000000000000000000 ) ) ;
#1322 = DIRECTION ( 'NONE',  ( -1.000000000000000000, -0.000000000000000000, -0.000000000000000000 ) ) ;
#1323 = AXIS2_PLACEMENT_3D ( 'NONE', #1066, #6909, #2148 ) ;
#1324 = DIRECTION ( 'NONE',  ( 0.000000000000000000, 0.000000000000000000, 1.000000000000000000 ) ) ;
#1325 = CARTESIAN_POINT ( 'NONE',  ( 2.783069004973548921, -5.408431875071614492, 23.92277630352793238 ) ) ;
#1326 = CIRCLE ( 'NONE', #12616, 31.62277660168379256 ) ;
#1327 = AXIS2_PLACEMENT_3D ( 'NONE', #8141, #12532, #6625 ) ;
#1328 = ORIENTED_EDGE ( 'NONE', *, *, #3928, .F. ) ;
#1329 = DIRECTION ( 'NONE',  ( 0.000000000000000000, 0.000000000000000000, 1.000000000000000000 ) ) ;
#1330 = CARTESIAN_POINT ( 'NONE',  ( 0.02531912748631555063, 2.311161484776756758, -14.46287784598614756 ) ) ;
#1331 = ORIENTED_EDGE ( 'NONE', *, *, #249, .F. ) ;
#1332 = DIRECTION ( 'NONE',  ( -0.000000000000000000, -0.000000000000000000, 1.000000000000000000 ) ) ;
#1333 = EDGE_LOOP ( 'NONE', ( #5720, #12557, #14675, #8271, #7245, #5481, #849 ) ) ;
#1334 = ORIENTED_EDGE ( 'NONE', *, *, #7370, .T. ) ;
#1335 = CARTESIAN_POINT ( 'NONE',  ( 80.00000000000000000, 0.000000000000000000, 4.500000000000000888 ) ) ;
#1337 = CARTESIAN_POINT ( 'NONE',  ( 2.789999999999999147, 12.59161484032942901, -21.30679549418617924 ) ) ;
#1336 = VECTOR ( 'NONE', #4511, 1000.000000000000000 ) ;
#1338 = AXIS2_PLACEMENT_3D ( 'NONE', #9790, #10088, #14487 ) ;
#1339 = VECTOR ( 'NONE', #483, 1000.000000000000000 ) ;
#1340 = CARTESIAN_POINT ( 'NONE',  ( 2.789999999999999147, 13.87420763704361093, 1.948757464274220697 ) ) ;
#1341 = DIRECTION ( 'NONE',  ( -1.000000000000000000, -0.000000000000000000, 0.000000000000000000 ) ) ;
#1342 = DIRECTION ( 'NONE',  ( -0.000000000000000000, -0.000000000000000000, 1.000000000000000000 ) ) ;
#1343 = ADVANCED_FACE ( 'NONE', ( #7786, #14944 ), #12543, .T. ) ;
#1344 = DIRECTION ( 'NONE',  ( -1.000000000000000000, -0.000000000000000000, -0.000000000000000000 ) ) ;
#1345 = ORIENTED_EDGE ( 'NONE', *, *, #9712, .T. ) ;
#1346 = CARTESIAN_POINT ( 'NONE',  ( 18.40394475573011945, -10.79473832354794460, 6.000000000000000000 ) ) ;
#1347 = LINE ( 'NONE', #10731, #35 ) ;
#1348 = AXIS2_PLACEMENT_3D ( 'NONE', #11884, #8204, #12885 ) ;
#1349 = DIRECTION ( 'NONE',  ( 0.000000000000000000, -1.000000000000000000, 0.000000000000000000 ) ) ;
#1350 = CIRCLE ( 'NONE', #11659, 2.524999999999996358 ) ;
#1351 = CARTESIAN_POINT ( 'NONE',  ( -10.00000000000000000, 0.000000000000000000, 0.000000000000000000 ) ) ;
#1352 = ORIENTED_EDGE ( 'NONE', *, *, #13563, .T. ) ;
#1353 = CIRCLE ( 'NONE', #6761, 4.000000000000000000 ) ;
#1354 = ORIENTED_EDGE ( 'NONE', *, *, #15079, .F. ) ;
#1355 = ORIENTED_EDGE ( 'NONE', *, *, #11067, .T. ) ;
#1356 = CARTESIAN_POINT ( 'NONE',  ( 1.039999999999997593, 0.000000000000000000, 0.000000000000000000 ) ) ;
#1357 = DIRECTION ( 'NONE',  ( -0.000000000000000000, -0.000000000000000000, -1.000000000000000000 ) ) ;
#1358 = CARTESIAN_POINT ( 'NONE',  ( 88.84370878116858705, 10.64188714589527507, -2.000000000000000888 ) ) ;
#1359 = CARTESIAN_POINT ( 'NONE',  ( -14.40394475573012301, -13.79473832354794993, 16.99999999999999645 ) ) ;
#1360 = DIRECTION ( 'NONE',  ( -1.000000000000000000, 0.000000000000000000, 0.000000000000000000 ) ) ;
#1361 = LINE ( 'NONE', #2683, #9152 ) ;
#1362 = AXIS2_PLACEMENT_3D ( 'NONE', #1099, #6945, #14485 ) ;
#1363 = AXIS2_PLACEMENT_3D ( 'NONE', #789, #12619, #15020 ) ;
#1364 = ORIENTED_EDGE ( 'NONE', *, *, #11141, .T. ) ;
#1365 = CARTESIAN_POINT ( 'NONE',  ( 0.9999999999999997780, -6.008326913195983998, -0.8000000000000000444 ) ) ;
#1366 = CARTESIAN_POINT ( 'NONE',  ( -20.63749999999999929, 0.000000000000000000, 0.000000000000000000 ) ) ;
#1367 = EDGE_LOOP ( 'NONE', ( #7183, #13097, #9718, #13636 ) ) ;
#1368 = CYLINDRICAL_SURFACE ( 'NONE', #5612, 2.524999999999999467 ) ;
#1369 = CARTESIAN_POINT ( 'NONE',  ( 0.000000000000000000, 0.000000000000000000, 5.500000000000000000 ) ) ;
#1370 = EDGE_CURVE ( 'NONE', #13796, #1588, #6008, .T. ) ;
#1371 = PRODUCT_DEFINITION_SHAPE ( 'NONE', 'NONE',  #15238 ) ;
#1372 = CARTESIAN_POINT ( 'NONE',  ( 0.8291131470075020493, -24.44424927289185590, 12.96989951879399072 ) ) ;
#1373 = VERTEX_POINT ( 'NONE', #9323 ) ;
#1374 = CIRCLE ( 'NONE', #2365, 2.447112362156698140 ) ;
#1375 = ORIENTED_EDGE ( 'NONE', *, *, #4711, .T. ) ;
#1376 = AXIS2_PLACEMENT_3D ( 'NONE', #7353, #6187, #9640 ) ;
#1377 = ORIENTED_EDGE ( 'NONE', *, *, #5249, .T. ) ;
#1378 = VERTEX_POINT ( 'NONE', #3404 ) ;
#1379 = B_SPLINE_CURVE_WITH_KNOTS ( 'NONE', 3,
 ( #3174, #6631, #853, #13696, #10459, #10232, #7861, #11529 ),
 .UNSPECIFIED., .F., .F.,
 ( 4, 2, 2, 4 ),
 ( 2.445728210258510103E-07, 0.001895260649874686140, 0.002842768688401514036, 0.003790276726928342148 ),
 .UNSPECIFIED. ) ;
#1380 = CARTESIAN_POINT ( 'NONE',  ( 0.000000000000000000, 1.991882183130315953, 24.04302995059967074 ) ) ;
#1381 = PRODUCT_DEFINITION ( 'UNKNOWN', '', #8671, #12385 ) ;
#1382 = DIRECTION ( 'NONE',  ( -0.000000000000000000, -0.000000000000000000, 1.000000000000000000 ) ) ;
#1383 = EDGE_CURVE ( 'NONE', #7996, #7166, #13791, .T. ) ;
#1384 = EDGE_CURVE ( 'NONE', #1805, #14461, #7483, .T. ) ;
#1385 = DIRECTION ( 'NONE',  ( 1.000000000000000000, 0.000000000000000000, 0.000000000000000000 ) ) ;
#1386 = CARTESIAN_POINT ( 'NONE',  ( 0.02436607992776151574, -16.37294372382871188, 18.55949924794887096 ) ) ;
#1387 = CIRCLE ( 'NONE', #5569, 2.524999999999999023 ) ;
#1388 = DIRECTION ( 'NONE',  ( 0.000000000000000000, 0.000000000000000000, 1.000000000000000000 ) ) ;
#1389 = AXIS2_PLACEMENT_3D ( 'NONE', #636, #4027, #8788 ) ;
#1390 = VERTEX_POINT ( 'NONE', #5491 ) ;
#1391 = DIRECTION ( 'NONE',  ( 0.000000000000000000, 0.000000000000000000, -1.000000000000000000 ) ) ;
#1392 = AXIS2_PLACEMENT_3D ( 'NONE', #12930, #7026, #11705 ) ;
#1393 = EDGE_CURVE ( 'NONE', #11633, #7557, #3313, .T. ) ;
#1394 = EDGE_CURVE ( 'NONE', #5482, #4132, #14540, .T. ) ;
#1395 = VECTOR ( 'NONE', #11283, 1000.000000000000000 ) ;
#1396 = ORIENTED_EDGE ( 'NONE', *, *, #2874, .T. ) ;
#1397 = CARTESIAN_POINT ( 'NONE',  ( 2.789999999999999147, 0.000000000000000000, 0.000000000000000000 ) ) ;
#1398 = CARTESIAN_POINT ( 'NONE',  ( 0.02531912748464631296, -13.68080036884344963, -5.229914364928496262 ) ) ;
#1399 = EDGE_CURVE ( 'NONE', #6697, #5334, #782, .T. ) ;
#1400 = VERTEX_POINT ( 'NONE', #4413 ) ;
#1401 = ORIENTED_EDGE ( 'NONE', *, *, #5062, .F. ) ;
#1402 = VECTOR ( 'NONE', #4636, 1000.000000000000000 ) ;
#1403 = AXIS2_PLACEMENT_3D ( 'NONE', #1515, #9820, #3977 ) ;
#1404 = CIRCLE ( 'NONE', #13462, 4.000000000000000000 ) ;
#1405 = DIRECTION ( 'NONE',  ( -1.000000000000000000, 0.000000000000000000, -0.000000000000000000 ) ) ;
#1406 = B_SPLINE_CURVE_WITH_KNOTS ( 'NONE', 3,
 ( #14050, #3453, #8069, #14211 ),
 .UNSPECIFIED., .F., .F.,
 ( 4, 4 ),
 ( 0.005123713096549377226, 0.005814346476695811915 ),
 .UNSPECIFIED. ) ;
#1407 = ADVANCED_FACE ( 'NONE', ( #862 ), #10161, .F. ) ;
#1408 = ORIENTED_EDGE ( 'NONE', *, *, #1194, .F. ) ;
#1409 = CARTESIAN_POINT ( 'NONE',  ( 0.000000000000000000, 1.948757464274368578, -13.87420763704359494 ) ) ;
#1410 = CARTESIAN_POINT ( 'NONE',  ( 2.508169649284527125, -15.84037596932105707, -3.072260951847695765 ) ) ;
#1411 = CARTESIAN_POINT ( 'NONE',  ( 80.00000000000000000, 0.000000000000000000, 3.000000000000002665 ) ) ;
#1412 = DIRECTION ( 'NONE',  ( -0.9988110320138940956, -0.04874958797097371510, 0.000000000000000000 ) ) ;
#1413=STYLED_ITEM('',(#15258),#13940);
#1414 = ORIENTED_EDGE ( 'NONE', *, *, #6168, .F. ) ;
#1415 = CIRCLE ( 'NONE', #4364, 2.524999999999995914 ) ;
#1416 = LINE ( 'NONE', #9630, #267 ) ;
#1417 = CARTESIAN_POINT ( 'NONE',  ( 1.039999999999996261, 12.96210679857786197, 24.89775460606836788 ) ) ;
#1418 = VECTOR ( 'NONE', #11737, 1000.000000000000000 ) ;
#1419 = AXIS2_PLACEMENT_3D ( 'NONE', #9521, #10244, #11889 ) ;
#1420 = VERTEX_POINT ( 'NONE', #4329 ) ;
#1421 = DIRECTION ( 'NONE',  ( 1.000000000000000000, 0.000000000000000000, 0.000000000000000000 ) ) ;
#1422 = ORIENTED_EDGE ( 'NONE', *, *, #790, .T. ) ;
#1423 = VERTEX_POINT ( 'NONE', #12766 ) ;
#1424 = DIRECTION ( 'NONE',  ( 1.000000000000000000, 0.000000000000000000, -0.000000000000000000 ) ) ;
#1425 = LINE ( 'NONE', #5277, #6096 ) ;
#1426 = DIRECTION ( 'NONE',  ( 0.000000000000000000, 0.000000000000000000, -1.000000000000000000 ) ) ;
#1427 = CARTESIAN_POINT ( 'NONE',  ( 0.5321745407694753460, 4.993157874728185952, -26.58873630738046501 ) ) ;
#1428 = LINE ( 'NONE', #8483, #6858 ) ;
#1429 = AXIS2_PLACEMENT_3D ( 'NONE', #14450, #12280, #8594 ) ;
#1430 = DIRECTION ( 'NONE',  ( 0.000000000000000000, 0.000000000000000000, 1.000000000000000000 ) ) ;
#1431 = AXIS2_PLACEMENT_3D ( 'NONE', #92, #11853, #9271 ) ;
#1432 = VERTEX_POINT ( 'NONE', #8007 ) ;
#1433 = CARTESIAN_POINT ( 'NONE',  ( 1.885839510111769979, -4.928563447326406610, 17.01651022436361771 ) ) ;
#1434 = DIRECTION ( 'NONE',  ( 0.000000000000000000, 0.000000000000000000, 1.000000000000000000 ) ) ;
#1435 = CARTESIAN_POINT ( 'NONE',  ( -19.40394475573011590, -4.794738323547945491, 12.00000000000000000 ) ) ;
#1436 = CARTESIAN_POINT ( 'NONE',  ( 0.000000000000000000, -15.04425356660774682, 20.70663861606266209 ) ) ;
#1437 = ORIENTED_EDGE ( 'NONE', *, *, #3878, .F. ) ;
#1438 = ORIENTED_EDGE ( 'NONE', *, *, #5807, .F. ) ;
#1439 = VERTEX_POINT ( 'NONE', #5711 ) ;
#1440 = VECTOR ( 'NONE', #1301, 1000.000000000000114 ) ;
#1441 = AXIS2_PLACEMENT_3D ( 'NONE', #14034, #11793, #15127 ) ;
#1442 = CARTESIAN_POINT ( 'NONE',  ( 0.5321745326902582729, -26.83036154824997155, 3.467596033028195635 ) ) ;
#1443 = LINE ( 'NONE', #3512, #4366 ) ;
#1444 = EDGE_CURVE ( 'NONE', #6713, #2082, #10507, .T. ) ;
#1445 = CARTESIAN_POINT ( 'NONE',  ( 67.23404255319145761, 28.93147646537025963, 7.000000000000000000 ) ) ;
#1446 = CARTESIAN_POINT ( 'NONE',  ( 2.765633920072237295, 12.59161484032912171, 21.30679549418635688 ) ) ;
#1447 = DIRECTION ( 'NONE',  ( -5.339417856040273846E-17, -1.063174570779084847E-17, 1.000000000000000000 ) ) ;
#1448 = CARTESIAN_POINT ( 'NONE',  ( 1.749999999999999778, 4.835383649608716361, -17.29145405592683815 ) ) ;
#1449 = ORIENTED_EDGE ( 'NONE', *, *, #14328, .F. ) ;
#1450 = CARTESIAN_POINT ( 'NONE',  ( 1.039999999999997593, 0.000000000000000000, 0.000000000000000000 ) ) ;
#1451 = CARTESIAN_POINT ( 'NONE',  ( 2.790000000000060876, 11.12234047011190263, 8.842064619038561446 ) ) ;
#1452 = EDGE_LOOP ( 'NONE', ( #12989, #5324, #2411, #6833, #11094 ) ) ;
#1453 = CARTESIAN_POINT ( 'NONE',  ( 74.00000000000000000, 0.000000000000000000, 5.500000000000000000 ) ) ;
#1454 = CARTESIAN_POINT ( 'NONE',  ( 2.257825459230522913, 26.58873630738059290, -4.993157874727537582 ) ) ;
#1455 = AXIS2_PLACEMENT_3D ( 'NONE', #11857, #7631, #8405 ) ;
#1456 = FACE_OUTER_BOUND ( 'NONE', #5574, .T. ) ;
#1457 = EDGE_CURVE ( 'NONE', #7167, #13302, #8454, .T. ) ;
#1458 = ORIENTED_EDGE ( 'NONE', *, *, #5920, .T. ) ;
#1459 = EDGE_CURVE ( 'NONE', #9282, #1757, #10468, .T. ) ;
#1460 = CARTESIAN_POINT ( 'NONE',  ( 1.749999999999999778, 17.39253030560841395, -4.458161950358560333 ) ) ;
#1461 = ORIENTED_EDGE ( 'NONE', *, *, #12060, .F. ) ;
#1462 = ORIENTED_EDGE ( 'NONE', *, *, #4915, .T. ) ;
#1463 = ORIENTED_EDGE ( 'NONE', *, *, #915, .T. ) ;
#1464 = DIRECTION ( 'NONE',  ( 0.000000000000000000, 0.000000000000000000, 1.000000000000000000 ) ) ;
#1465 = CARTESIAN_POINT ( 'NONE',  ( -20.63749999999999929, 0.000000000000000000, -4.424999999999999822 ) ) ;
#1466 = B_SPLINE_CURVE_WITH_KNOTS ( 'NONE', 3,
 ( #796, #4196, #13559, #2103, #5501, #7719 ),
 .UNSPECIFIED., .F., .F.,
 ( 4, 2, 4 ),
 ( 2.321268216997199256E-07, 0.001878622960950494455, 0.003757013795079288884 ),
 .UNSPECIFIED. ) ;
#1467 = ADVANCED_FACE ( 'NONE', ( #6862 ), #9694, .T. ) ;
#1468 = DIRECTION ( 'NONE',  ( 0.000000000000000000, 0.000000000000000000, 1.000000000000000000 ) ) ;
#1469 = CARTESIAN_POINT ( 'NONE',  ( 80.00000000000000000, -9.999999999999994671, -131.1575142076926852 ) ) ;
#1470 = DIRECTION ( 'NONE',  ( 0.000000000000000000, 0.000000000000000000, -1.000000000000000000 ) ) ;
#1471 = CARTESIAN_POINT ( 'NONE',  ( 2.789999999999999147, 0.000000000000000000, 0.000000000000000000 ) ) ;
#1472 = ORIENTED_EDGE ( 'NONE', *, *, #5616, .F. ) ;
#1473 = DIRECTION ( 'NONE',  ( 1.000000000000000000, 0.000000000000000000, 0.000000000000000000 ) ) ;
#1474 = ADVANCED_FACE ( 'NONE', ( #3181 ), #9091, .F. ) ;
#1475 = EDGE_CURVE ( 'NONE', #7248, #11593, #5936, .T. ) ;
#1476 = TOROIDAL_SURFACE ( 'NONE', #10070, 5.899999999999999467, 0.1000000000000010186 ) ;
#1477 = ORIENTED_EDGE ( 'NONE', *, *, #1540, .F. ) ;
#1478 = EDGE_LOOP ( 'NONE', ( #3332, #9837, #9394, #9371, #9412, #4981 ) ) ;
#1479 = CARTESIAN_POINT ( 'NONE',  ( 1.039999999999995817, 27.76164181293051669, 4.147968289691385202 ) ) ;
#1480 = FACE_OUTER_BOUND ( 'NONE', #4378, .T. ) ;
#1481 = EDGE_LOOP ( 'NONE', ( #11695, #14531, #10098, #7397 ) ) ;
#1482 = VERTEX_POINT ( 'NONE', #8309 ) ;
#1483 = CARTESIAN_POINT ( 'NONE',  ( 0.000000000000000000, 0.000000000000000000, 0.000000000000000000 ) ) ;
#1484 = EDGE_CURVE ( 'NONE', #10057, #393, #5096, .T. ) ;
#1485 = VERTEX_POINT ( 'NONE', #10550 ) ;
#1486 = CARTESIAN_POINT ( 'NONE',  ( 80.00000000000000000, -9.999999999999994671, 7.000000000000000000 ) ) ;
#1487 = CARTESIAN_POINT ( 'NONE',  ( 0.02436607992775978102, 2.336989772644613161, -24.63872515616080250 ) ) ;
#1488 = EDGE_CURVE ( 'NONE', #5963, #15052, #13663, .T. ) ;
#1489 = EDGE_CURVE ( 'NONE', #12388, #13917, #12187, .T. ) ;
#1490 = LINE ( 'NONE', #1557, #4783 ) ;
#1491 = ORIENTED_EDGE ( 'NONE', *, *, #1285, .T. ) ;
#1492 = CARTESIAN_POINT ( 'NONE',  ( 2.257825467309741541, 3.467596033028661928, -26.83036154824990760 ) ) ;
#1493 = DIRECTION ( 'NONE',  ( -0.4036950204470279302, 0.9148936170212763619, 0.000000000000000000 ) ) ;
#1494 = ORIENTED_EDGE ( 'NONE', *, *, #4486, .F. ) ;
#1495 = CARTESIAN_POINT ( 'NONE',  ( 0.1920562174424405855, 12.05486625177571547, 10.28947301956286431 ) ) ;
#1496 = CYLINDRICAL_SURFACE ( 'NONE', #8697, 4.872650870659752442 ) ;
#1497 = ORIENTED_EDGE ( 'NONE', *, *, #6234, .F. ) ;
#1498 = ORIENTED_EDGE ( 'NONE', *, *, #12801, .T. ) ;
#1499 = FACE_OUTER_BOUND ( 'NONE', #2066, .T. ) ;
#1500 = LINE ( 'NONE', #12168, #14620 ) ;
#1501 = CARTESIAN_POINT ( 'NONE',  ( 0.000000000000000000, 20.62201879784932856, -12.52067188844328705 ) ) ;
#1502 = DIRECTION ( 'NONE',  ( 0.000000000000000000, 0.000000000000000000, 1.000000000000000000 ) ) ;
#1504 = VERTEX_POINT ( 'NONE', #14151 ) ;
#1503 = EDGE_CURVE ( 'NONE', #7572, #3527, #300, .T. ) ;
#1505 = PLANE ( 'NONE',  #15194 ) ;
#1506 = CARTESIAN_POINT ( 'NONE',  ( 13.94557569532858032, -25.06424573764405395, 5.000000000000000000 ) ) ;
#1507 = CARTESIAN_POINT ( 'NONE',  ( 2.789999999999999147, -8.936381166381891568E-14, 25.59481291497571220 ) ) ;
#1508 = CARTESIAN_POINT ( 'NONE',  ( 2.789999999999999147, 14.19996452731195546, -4.595504208219880482 ) ) ;
#1509 = ORIENTED_EDGE ( 'NONE', *, *, #4495, .T. ) ;
#1510 = VERTEX_POINT ( 'NONE', #11832 ) ;
#1511 = ADVANCED_FACE ( 'NONE', ( #9456 ), #12987, .T. ) ;
#1512 = ORIENTED_EDGE ( 'NONE', *, *, #2860, .T. ) ;
#1513 = FACE_OUTER_BOUND ( 'NONE', #3682, .T. ) ;
#1514 = DIRECTION ( 'NONE',  ( -1.000000000000000000, -0.000000000000000000, -0.000000000000000000 ) ) ;
#1515 = CARTESIAN_POINT ( 'NONE',  ( 2.789999999999999147, -23.31896751603337137, 7.334849878007427826 ) ) ;
#1516 = CARTESIAN_POINT ( 'NONE',  ( 1.749999999999999778, 4.458161950358745074, -17.39253030560836777 ) ) ;
#1517 =( LENGTH_UNIT ( ) NAMED_UNIT ( * ) SI_UNIT ( .MILLI., .METRE. ) );
#1518 = DIRECTION ( 'NONE',  ( -0.000000000000000000, -0.000000000000000000, 1.000000000000000000 ) ) ;
#1519 = VERTEX_POINT ( 'NONE', #5 ) ;
#1520 = CARTESIAN_POINT ( 'NONE',  ( -2.321707774797442170, -4.824281976789052351, -0.8000000000000000444 ) ) ;
#1521 = DIRECTION ( 'NONE',  ( 0.000000000000000000, 0.000000000000000000, 1.000000000000000000 ) ) ;
#1522 = ORIENTED_EDGE ( 'NONE', *, *, #12181, .T. ) ;
#1523 = DIRECTION ( 'NONE',  ( 1.000000000000000000, 0.000000000000000000, 0.000000000000000000 ) ) ;
#1524 = VECTOR ( 'NONE', #2212, 1000.000000000000000 ) ;
#1525 = LINE ( 'NONE', #9830, #6536 ) ;
#1526 = DIRECTION ( 'NONE',  ( 0.000000000000000000, 0.000000000000000000, 1.000000000000000000 ) ) ;
#1527 = EDGE_CURVE ( 'NONE', #14446, #9599, #1641, .T. ) ;
#1528 = VERTEX_POINT ( 'NONE', #10692 ) ;
#1529 = LINE ( 'NONE', #7454, #4580 ) ;
#1530 = LINE ( 'NONE', #9835, #380 ) ;
#1531 = ORIENTED_EDGE ( 'NONE', *, *, #3062, .T. ) ;
#1532 = EDGE_LOOP ( 'NONE', ( #3117, #4460, #13209, #9461, #14696 ) ) ;
#1533 = EDGE_LOOP ( 'NONE', ( #3960, #14213, #11513, #14850 ) ) ;
#1534 = CARTESIAN_POINT ( 'NONE',  ( 0.9999999999999997780, -6.008326913195983998, -0.8000000000000000444 ) ) ;
#1535 = AXIS2_PLACEMENT_3D ( 'NONE', #15062, #1284, #13903 ) ;
#1536 = CARTESIAN_POINT ( 'NONE',  ( 2.718131885465892239, 16.91241718341998634, 18.89333555428560274 ) ) ;
#1537 = B_SPLINE_CURVE_WITH_KNOTS ( 'NONE', 3,
 ( #2299, #14055, #8211, #14291 ),
 .UNSPECIFIED., .F., .F.,
 ( 4, 4 ),
 ( 2.034713381942770827E-07, 0.0006887909409525120848 ),
 .UNSPECIFIED. ) ;
#1538 = LINE ( 'NONE', #4939, #7482 ) ;
#1539 = CARTESIAN_POINT ( 'NONE',  ( 10.00000000000000178, -1.390791565672601315, 3.000000000000002665 ) ) ;
#1540 = EDGE_CURVE ( 'NONE', #14414, #5535, #6005, .T. ) ;
#1541 = CARTESIAN_POINT ( 'NONE',  ( 1.039999999999997593, 0.000000000000000000, 0.000000000000000000 ) ) ;
#1542 =( REPRESENTATION_RELATIONSHIP ('NONE','NONE', #12685, #14263 ) REPRESENTATION_RELATIONSHIP_WITH_TRANSFORMATION ( #15044 )SHAPE_REPRESENTATION_RELATIONSHIP( ) );
#1543 = EDGE_CURVE ( 'NONE', #8254, #761, #13055, .T. ) ;
#1544 = ORIENTED_EDGE ( 'NONE', *, *, #12438, .F. ) ;
#1545 = DIRECTION ( 'NONE',  ( 0.000000000000000000, 0.000000000000000000, 1.000000000000000000 ) ) ;
#1546 =( LENGTH_UNIT ( ) NAMED_UNIT ( * ) SI_UNIT ( .MILLI., .METRE. ) );
#1547 = VERTEX_POINT ( 'NONE', #11683 ) ;
#1548 = ORIENTED_EDGE ( 'NONE', *, *, #7466, .F. ) ;
#1549 = DIRECTION ( 'NONE',  ( -1.000000000000000000, -0.000000000000000000, -0.000000000000000000 ) ) ;
#1550 = DIRECTION ( 'NONE',  ( -0.9873505073845698643, 0.1585527532634883330, -5.103307673902845341E-17 ) ) ;
#1551 = EDGE_LOOP ( 'NONE', ( #3528, #541, #2755, #9080, #10467 ) ) ;
#1552 = CARTESIAN_POINT ( 'NONE',  ( 0.02436607992776628623, 24.63872515616082737, -2.336989772644355590 ) ) ;
#1553 = ORIENTED_EDGE ( 'NONE', *, *, #8444, .F. ) ;
#1554 = FACE_OUTER_BOUND ( 'NONE', #1889, .T. ) ;
#1555 = CYLINDRICAL_SURFACE ( 'NONE', #6355, 5.575000000000000178 ) ;
#1556 = B_SPLINE_CURVE_WITH_KNOTS ( 'NONE', 3,
 ( #690, #4387, #4304, #13594 ),
 .UNSPECIFIED., .F., .F.,
 ( 4, 4 ),
 ( 0.005258120783916789796, 0.005948386350302922905 ),
 .UNSPECIFIED. ) ;
#1557 = CARTESIAN_POINT ( 'NONE',  ( -14.40394475573012301, -4.794738323547945491, 19.99999999999999645 ) ) ;
#1558 = EDGE_CURVE ( 'NONE', #2099, #14023, #9734, .T. ) ;
#1559 = ORIENTED_EDGE ( 'NONE', *, *, #5818, .T. ) ;
#1560 = DIRECTION ( 'NONE',  ( 1.000000000000000000, 0.000000000000000000, 0.000000000000000000 ) ) ;
#1561 = LINE ( 'NONE', #480, #145 ) ;
#1562 = ORIENTED_EDGE ( 'NONE', *, *, #1939, .T. ) ;
#1563 = DIRECTION ( 'NONE',  ( -1.000000000000000000, -0.000000000000000000, 0.000000000000000000 ) ) ;
#1564 = DIRECTION ( 'NONE',  ( -1.000000000000000000, -0.000000000000000000, 0.000000000000000000 ) ) ;
#1565 = VERTEX_POINT ( 'NONE', #14306 ) ;
#1566 = VERTEX_POINT ( 'NONE', #10772 ) ;
#1567 =( NAMED_UNIT ( * ) PLANE_ANGLE_UNIT ( ) SI_UNIT ( $, .RADIAN. ) );
#1568 = CARTESIAN_POINT ( 'NONE',  ( 85.79342132543153809, 17.83186255874426962, 4.000000000000000000 ) ) ;
#1569 = EDGE_CURVE ( 'NONE', #883, #13931, #1171, .T. ) ;
#1570 = EDGE_CURVE ( 'NONE', #2216, #4678, #12832, .T. ) ;
#1571 = EDGE_CURVE ( 'NONE', #13989, #10279, #3470, .T. ) ;
#1572 = PRESENTATION_STYLE_ASSIGNMENT (( #328 ) ) ;
#1573 = FACE_OUTER_BOUND ( 'NONE', #3157, .T. ) ;
#1574 = AXIS2_PLACEMENT_3D ( 'NONE', #13243, #10929, #13389 ) ;
#1575 = DIRECTION ( 'NONE',  ( -1.000000000000000000, 0.000000000000000000, -0.000000000000000000 ) ) ;
#1576 = AXIS2_PLACEMENT_3D ( 'NONE', #10565, #9261, #17 ) ;
#1577 = VERTEX_POINT ( 'NONE', #3538 ) ;
#1578 = PLANE ( 'NONE',  #2664 ) ;
#1579 = DIRECTION ( 'NONE',  ( 0.000000000000000000, 0.000000000000000000, -1.000000000000000000 ) ) ;
#1580 = CARTESIAN_POINT ( 'NONE',  ( 2.789999999999999147, -15.04425356660744839, -20.70663861606288236 ) ) ;
#1581 = PRESENTATION_STYLE_ASSIGNMENT (( #7433 ) ) ;
#1582 = VERTEX_POINT ( 'NONE', #3767 ) ;
#1583 = EDGE_CURVE ( 'NONE', #12872, #5857, #2627, .T. ) ;
#1584 = ORIENTED_EDGE ( 'NONE', *, *, #11111, .T. ) ;
#1585 = TOROIDAL_SURFACE ( 'NONE', #6489, 24.12539914357697768, 8.000000000000000000 ) ;
#1586 = EDGE_CURVE ( 'NONE', #13319, #1997, #3119, .T. ) ;
#1587 = AXIS2_PLACEMENT_3D ( 'NONE', #4100, #5260, #8780 ) ;
#1588 = VERTEX_POINT ( 'NONE', #12905 ) ;
#1589 = VECTOR ( 'NONE', #7529, 1000.000000000000000 ) ;
#1590 = CARTESIAN_POINT ( 'NONE',  ( 0.7592463941534255412, -27.31305418910211813, 3.797885586973120287 ) ) ;
#1591 = DIRECTION ( 'NONE',  ( 0.000000000000000000, 0.000000000000000000, 1.000000000000000000 ) ) ;
#1592 = EDGE_CURVE ( 'NONE', #8603, #8358, #5211, .T. ) ;
#1593 = B_SPLINE_CURVE_WITH_KNOTS ( 'NONE', 3,
 ( #11439, #14838, #12594, #3081 ),
 .UNSPECIFIED., .F., .F.,
 ( 4, 4 ),
 ( 2.451234579310872104E-07, 0.0006917187676826492410 ),
 .UNSPECIFIED. ) ;
#1594 = CARTESIAN_POINT ( 'NONE',  ( 0.000000000000000000, -5.249430348645662825, -12.98979500319700264 ) ) ;
#1595 = CARTESIAN_POINT ( 'NONE',  ( 0.000000000000000000, 0.000000000000000000, 10.00000000000000000 ) ) ;
#1596 = CARTESIAN_POINT ( 'NONE',  ( 0.000000000000000000, 0.000000000000000000, 0.000000000000000000 ) ) ;
#1597 = CARTESIAN_POINT ( 'NONE',  ( 2.440610831926789182, 15.53033051714692014, 5.240368680323600259 ) ) ;
#1598 =( GEOMETRIC_REPRESENTATION_CONTEXT ( 3 ) GLOBAL_UNCERTAINTY_ASSIGNED_CONTEXT ( ( #5190 ) ) GLOBAL_UNIT_ASSIGNED_CONTEXT ( ( #5513, #14057, #4970 ) ) REPRESENTATION_CONTEXT ( 'NONE', 'WORKASPACE' ) );
#1599 = ORIENTED_EDGE ( 'NONE', *, *, #10293, .T. ) ;
#1600 = CARTESIAN_POINT ( 'NONE',  ( 0.1855655959470677019, -19.17825124759764677, -17.45907811351477079 ) ) ;
#1601 = DIRECTION ( 'NONE',  ( 1.000000000000000000, 0.000000000000000000, 0.000000000000000000 ) ) ;
#1602 = VECTOR ( 'NONE', #10196, 1000.000000000000000 ) ;
#1603 = EDGE_CURVE ( 'NONE', #1860, #1482, #7085, .T. ) ;
#1604 = ORIENTED_EDGE ( 'NONE', *, *, #6490, .T. ) ;
#1605 = FACE_OUTER_BOUND ( 'NONE', #6436, .T. ) ;
#1606 = CARTESIAN_POINT ( 'NONE',  ( 1.823865745262398308, 24.74813374239829145, 12.96725027898200899 ) ) ;
#1607 = VECTOR ( 'NONE', #13853, 1000.000000000000000 ) ;
#1608 = B_SPLINE_CURVE_WITH_KNOTS ( 'NONE', 3,
 ( #9989, #1536, #7461, #6225, #9842, #12362 ),
 .UNSPECIFIED., .F., .F.,
 ( 4, 2, 4 ),
 ( 2.321268216997094965E-07, 0.001878622960950493588, 0.003757013795079287150 ),
 .UNSPECIFIED. ) ;
#1609 = CARTESIAN_POINT ( 'NONE',  ( 2.358581579527286198, -23.43037373958380343, 12.94152279942367656 ) ) ;
#1610 = ORIENTED_EDGE ( 'NONE', *, *, #10529, .F. ) ;
#1611 = DIRECTION ( 'NONE',  ( -0.000000000000000000, -1.000000000000000000, -0.000000000000000000 ) ) ;
#1612 = CARTESIAN_POINT ( 'NONE',  ( -7.634507448887241432E-14, 22.38018801136490055, -9.515416771310970745 ) ) ;
#1613 = ORIENTED_EDGE ( 'NONE', *, *, #13229, .T. ) ;
#1614 = ORIENTED_EDGE ( 'NONE', *, *, #8614, .F. ) ;
#1615 = ORIENTED_EDGE ( 'NONE', *, *, #12503, .F. ) ;
#1616 = LINE ( 'NONE', #686, #9254 ) ;
#1617 = AXIS2_PLACEMENT_3D ( 'NONE', #644, #5052, #5207 ) ;
#1618 = CARTESIAN_POINT ( 'NONE',  ( 0.02436607992776455150, 21.30679549418631780, 12.59161484032919986 ) ) ;
#1619 = CIRCLE ( 'NONE', #1856, 3.799999999999998934 ) ;
#1620 = DIRECTION ( 'NONE',  ( 1.000000000000000000, 0.000000000000000000, 0.000000000000000000 ) ) ;
#1621 = PLANE ( 'NONE',  #11146 ) ;
#1622 = DIRECTION ( 'NONE',  ( -1.000000000000000000, -0.000000000000000000, -0.000000000000000000 ) ) ;
#1623 = CARTESIAN_POINT ( 'NONE',  ( 1.749999999999999778, 12.55714665599987079, 12.83329210556836308 ) ) ;
#1624 = ORIENTED_EDGE ( 'NONE', *, *, #9442, .T. ) ;
#1625 = DIRECTION ( 'NONE',  ( 0.000000000000000000, 2.061057595219972332E-15, -1.000000000000000000 ) ) ;
#1626 = CIRCLE ( 'NONE', #5563, 17.95481323787947403 ) ;
#1627 = B_SPLINE_CURVE_WITH_KNOTS ( 'NONE', 3,
 ( #6678, #11358, #1995, #10355 ),
 .UNSPECIFIED., .F., .F.,
 ( 4, 4 ),
 ( 0.005258139959819237326, 0.005948405594583419317 ),
 .UNSPECIFIED. ) ;
#1628 = ORIENTED_EDGE ( 'NONE', *, *, #6271, .F. ) ;
#1629 = ORIENTED_EDGE ( 'NONE', *, *, #7674, .T. ) ;
#1630 = CARTESIAN_POINT ( 'NONE',  ( 0.000000000000000000, 22.25075486061737351, 9.324097380959511128 ) ) ;
#1631 = AXIS2_PLACEMENT_3D ( 'NONE', #2376, #11890, #11748 ) ;
#1632 = VERTEX_POINT ( 'NONE', #10996 ) ;
#1633 = AXIS2_PLACEMENT_3D ( 'NONE', #12047, #11057, #10829 ) ;
#1634 = UNCERTAINTY_MEASURE_WITH_UNIT (LENGTH_MEASURE( 1.000000000000000082E-05 ), #6541, 'distance_accuracy_value', 'NONE');
#1635 = DIRECTION ( 'NONE',  ( 0.000000000000000000, 0.000000000000000000, 1.000000000000000000 ) ) ;
#1636 = EDGE_LOOP ( 'NONE', ( #8758, #1159, #8999, #4436 ) ) ;
#1637 = LINE ( 'NONE', #14555, #13858 ) ;
#1638 = CARTESIAN_POINT ( 'NONE',  ( -20.63749999999999574, 0.000000000000000000, 0.000000000000000000 ) ) ;
#1639 = CARTESIAN_POINT ( 'NONE',  ( 2.789999999999999147, -5.404747904883309660E-14, 15.47981323787947794 ) ) ;
#1640 = VECTOR ( 'NONE', #1054, 1000.000000000000000 ) ;
#1641 = CIRCLE ( 'NONE', #6308, 4.999999999999997335 ) ;
#1642 = CARTESIAN_POINT ( 'NONE',  ( 0.02436607992776455150, 5.391175441198956086, -24.15498966839956907 ) ) ;
#1643 = DIRECTION ( 'NONE',  ( 0.04874958797097354163, -0.9988110320138942066, 0.000000000000000000 ) ) ;
#1644 = VECTOR ( 'NONE', #11061, 1000.000000000000000 ) ;
#1645 = ORIENTED_EDGE ( 'NONE', *, *, #13717, .T. ) ;
#1646 = VECTOR ( 'NONE', #5740, 1000.000000000000114 ) ;
#1647 = CYLINDRICAL_SURFACE ( 'NONE', #13911, 13.20000000000000107 ) ;
#1648 = EDGE_CURVE ( 'NONE', #7241, #13039, #7780, .T. ) ;
#1649 = CARTESIAN_POINT ( 'NONE',  ( 1.000000000000000000, -5.408326913195983465, -0.8000000000000000444 ) ) ;
#1650 = ORIENTED_EDGE ( 'NONE', *, *, #4884, .T. ) ;
#1651 = ORIENTED_EDGE ( 'NONE', *, *, #10497, .F. ) ;
#1652 = CARTESIAN_POINT ( 'NONE',  ( 0.000000000000000000, -9.324097380959594616, 22.25075486061734509 ) ) ;
#1653 = FACE_BOUND ( 'NONE', #6790, .T. ) ;
#1654 = EDGE_CURVE ( 'NONE', #9529, #3623, #15149, .T. ) ;
#1655 =( NAMED_UNIT ( * ) SI_UNIT ( $, .STERADIAN. ) SOLID_ANGLE_UNIT ( ) );
#1656 = CYLINDRICAL_SURFACE ( 'NONE', #1617, 13.19999999999999929 ) ;
#1657 = DIRECTION ( 'NONE',  ( 0.000000000000000000, 0.000000000000000000, 1.000000000000000000 ) ) ;
#1658 = COLOUR_RGB ( '',0.8941176470588234615, 0.8941176470588234615, 0.8941176470588234615 ) ;
#1659 = ORIENTED_EDGE ( 'NONE', *, *, #4604, .F. ) ;
#1660 = CARTESIAN_POINT ( 'NONE',  ( 2.337784068222785283, -5.191253194756122902, 15.84984805378629424 ) ) ;
#1661 = DIRECTION ( 'NONE',  ( 0.000000000000000000, 0.000000000000000000, 1.000000000000000000 ) ) ;
#1662 = AXIS2_PLACEMENT_3D ( 'NONE', #8352, #2747, #500 ) ;
#1663 = TOROIDAL_SURFACE ( 'NONE', #14929, 24.12539914357697768, 8.000000000000000000 ) ;
#1664 = DIRECTION ( 'NONE',  ( 0.7573544145849105957, -0.6530040510661073716, -2.081668171172162967E-17 ) ) ;
#1665 = CYLINDRICAL_SURFACE ( 'NONE', #14918, 13.19999999999999929 ) ;
#1666 = ADVANCED_FACE ( 'NONE', ( #5181 ), #2375, .T. ) ;
#1667 = EDGE_CURVE ( 'NONE', #6064, #9763, #575, .T. ) ;
#1668 = ORIENTED_EDGE ( 'NONE', *, *, #2242, .F. ) ;
#1669 = ORIENTED_EDGE ( 'NONE', *, *, #460, .T. ) ;
#1670 = EDGE_LOOP ( 'NONE', ( #5556, #3754, #10771, #4263 ) ) ;
#1671 = VECTOR ( 'NONE', #11024, 1000.000000000000000 ) ;
#1672 = CARTESIAN_POINT ( 'NONE',  ( 0.000000000000000000, 0.000000000000000000, 0.000000000000000000 ) ) ;
#1673 = CARTESIAN_POINT ( 'NONE',  ( 2.789999999999999147, -7.739906618939614624, -13.40591150984234581 ) ) ;
#1674 = AXIS2_PLACEMENT_3D ( 'NONE', #967, #4359, #11491 ) ;
#1675 = VECTOR ( 'NONE', #9164, 1000.000000000000227 ) ;
#1676 = CARTESIAN_POINT ( 'NONE',  ( 2.030753616560876829, -24.80264696524875490, -12.05220173035465336 ) ) ;
#1677 = FACE_OUTER_BOUND ( 'NONE', #7827, .T. ) ;
#1678 = FACE_OUTER_BOUND ( 'NONE', #14305, .T. ) ;
#1679 = CARTESIAN_POINT ( 'NONE',  ( 62.65957446808508280, 26.91300136313512681, -8.169391093593850073 ) ) ;
#1680 = CARTESIAN_POINT ( 'NONE',  ( 2.718131853594927261, 12.74240566899015903, -21.92302674874949986 ) ) ;
#1681 = EDGE_CURVE ( 'NONE', #15005, #6121, #9575, .T. ) ;
#1682 = ORIENTED_EDGE ( 'NONE', *, *, #11497, .T. ) ;
#1683 = DIRECTION ( 'NONE',  ( 1.000000000000000000, 0.000000000000000000, 0.000000000000000000 ) ) ;
#1684 = CARTESIAN_POINT ( 'NONE',  ( 2.764680872513933796, 5.229914364928542447, -13.68080036884343009 ) ) ;
#1685 = CARTESIAN_POINT ( 'NONE',  ( 85.79342132543153809, 17.83186255874426962, 6.000000000000000000 ) ) ;
#1686 = EDGE_CURVE ( 'NONE', #13918, #15033, #10957, .T. ) ;
#1687 = ORIENTED_EDGE ( 'NONE', *, *, #4711, .F. ) ;
#1688 = CIRCLE ( 'NONE', #8786, 2.524999999999999023 ) ;
#1689 = TOROIDAL_SURFACE ( 'NONE', #9051, 14.01039946648073986, 8.000000000000000000 ) ;
#1690 = DIRECTION ( 'NONE',  ( 0.000000000000000000, 0.000000000000000000, 1.000000000000000000 ) ) ;
#1691 = CARTESIAN_POINT ( 'NONE',  ( 0.02436607992776325046, -18.55949924794904504, 16.37294372382852004 ) ) ;
#1692 = ORIENTED_EDGE ( 'NONE', *, *, #1093, .F. ) ;
#1693 = ORIENTED_EDGE ( 'NONE', *, *, #9686, .T. ) ;
#1694 = DIRECTION ( 'NONE',  ( -5.339417856040273846E-17, -1.063174570779084847E-17, 1.000000000000000000 ) ) ;
#1695 = CARTESIAN_POINT ( 'NONE',  ( 0.000000000000000000, 0.000000000000000000, -0.8000000000000000444 ) ) ;
#1696 = EDGE_CURVE ( 'NONE', #6713, #2610, #6547, .T. ) ;
#1697 = CARTESIAN_POINT ( 'NONE',  ( 0.02436607992775978102, 2.336989772644613161, -24.63872515616080250 ) ) ;
#1698 = DIRECTION ( 'NONE',  ( 0.000000000000000000, 0.000000000000000000, 1.000000000000000000 ) ) ;
#1699 = CARTESIAN_POINT ( 'NONE',  ( -5.209999999999999964, 0.000000000000000000, 0.000000000000000000 ) ) ;
#1700 = CARTESIAN_POINT ( 'NONE',  ( 84.00000000000000000, 0.000000000000000000, 4.500000000000003553 ) ) ;
#1701 = AXIS2_PLACEMENT_3D ( 'NONE', #11946, #12178, #7362 ) ;
#1702 = ORIENTED_EDGE ( 'NONE', *, *, #7697, .F. ) ;
#1703 = LINE ( 'NONE', #8538, #10944 ) ;
#1704 = DIRECTION ( 'NONE',  ( 1.000000000000000000, 0.000000000000000000, 0.000000000000000000 ) ) ;
#1705 = SURFACE_STYLE_USAGE ( .BOTH. , #13375 ) ;
#1706 = ORIENTED_EDGE ( 'NONE', *, *, #3827, .F. ) ;
#1707 = ORIENTED_EDGE ( 'NONE', *, *, #7385, .T. ) ;
#1708 = ORIENTED_EDGE ( 'NONE', *, *, #4189, .F. ) ;
#1709 = AXIS2_PLACEMENT_3D ( 'NONE', #10548, #12901, #7081 ) ;
#1710 = CARTESIAN_POINT ( 'NONE',  ( 0.02531912748464674665, 11.36963888406700285, -9.232963481057645083 ) ) ;
#1711 = DIRECTION ( 'NONE',  ( 0.9988110320138940956, 0.04874958797097355551, -0.000000000000000000 ) ) ;
#1712 = EDGE_CURVE ( 'NONE', #4813, #13461, #899, .T. ) ;
#1713 = EDGE_LOOP ( 'NONE', ( #6464, #13973, #12040, #4774 ) ) ;
#1714 = B_SPLINE_CURVE_WITH_KNOTS ( 'NONE', 3,
 ( #5116, #2945, #627, #3951 ),
 .UNSPECIFIED., .F., .F.,
 ( 4, 4 ),
 ( 0.002880534149780423873, 0.003796793755617398208 ),
 .UNSPECIFIED. ) ;
#1715 = DIRECTION ( 'NONE',  ( -1.000000000000000000, 0.000000000000000000, -0.000000000000000000 ) ) ;
#1716 = ORIENTED_EDGE ( 'NONE', *, *, #6838, .T. ) ;
#1717 = DIRECTION ( 'NONE',  ( 0.9988110320138940956, 0.04874958797097354857, 0.000000000000000000 ) ) ;
#1718 = DIRECTION ( 'NONE',  ( 0.000000000000000000, 0.000000000000000000, 1.000000000000000000 ) ) ;
#1719 = VECTOR ( 'NONE', #8136, 1000.000000000000000 ) ;
#1720 = DIRECTION ( 'NONE',  ( -1.000000000000000000, -0.000000000000000000, 0.000000000000000000 ) ) ;
#1721 = CARTESIAN_POINT ( 'NONE',  ( 98.63205416320636232, -2.094184955359725375, 7.000000000000000000 ) ) ;
#1722 = ADVANCED_FACE ( 'NONE', ( #3853 ), #11070, .F. ) ;
#1723 = CARTESIAN_POINT ( 'NONE',  ( 0.5431870686475167576, 12.54666350726139790, -11.42270873787279761 ) ) ;
#1724 = VERTEX_POINT ( 'NONE', #7621 ) ;
#1725 = CARTESIAN_POINT ( 'NONE',  ( 56.98919079003883326, 3.953582723775848962, 2.999999999999999112 ) ) ;
#1726 = DIRECTION ( 'NONE',  ( 0.000000000000000000, 0.000000000000000000, 1.000000000000000000 ) ) ;
#1727 = ORIENTED_EDGE ( 'NONE', *, *, #13983, .T. ) ;
#1728 = ORIENTED_EDGE ( 'NONE', *, *, #15096, .F. ) ;
#1729 =( NAMED_UNIT ( * ) SI_UNIT ( $, .STERADIAN. ) SOLID_ANGLE_UNIT ( ) );
#1730 = CARTESIAN_POINT ( 'NONE',  ( 2.783025228907522131, -9.686319561461109728, 22.53337530003400246 ) ) ;
#1731 = CARTESIAN_POINT ( 'NONE',  ( 8.000000000000000000, 0.000000000000000000, 0.000000000000000000 ) ) ;
#1732 = EDGE_CURVE ( 'NONE', #3235, #9526, #15133, .T. ) ;
#1733 = LINE ( 'NONE', #5366, #10983 ) ;
#1734 = EDGE_CURVE ( 'NONE', #14461, #2630, #1703, .T. ) ;
#1735 = ORIENTED_EDGE ( 'NONE', *, *, #3302, .F. ) ;
#1736 = CARTESIAN_POINT ( 'NONE',  ( 2.597943565934061727, -5.295083827234814855, 14.93837896275547905 ) ) ;
#1737 = DIRECTION ( 'NONE',  ( 0.000000000000000000, -0.000000000000000000, 1.000000000000000000 ) ) ;
#1738 = CYLINDRICAL_SURFACE ( 'NONE', #12242, 8.400000000000000355 ) ;
#1739 = CARTESIAN_POINT ( 'NONE',  ( 1.039999999999996483, 17.39253030560841395, 4.458161950358563885 ) ) ;
#1740 = ORIENTED_EDGE ( 'NONE', *, *, #12994, .T. ) ;
#1741 = B_SPLINE_CURVE_WITH_KNOTS ( 'NONE', 3,
 ( #7225, #13048, #4937, #12897 ),
 .UNSPECIFIED., .F., .F.,
 ( 4, 4 ),
 ( 1.981826382900813409E-07, 0.0006887856082032219702 ),
 .UNSPECIFIED. ) ;
#1742 = VERTEX_POINT ( 'NONE', #7398 ) ;
#1743 = VERTEX_POINT ( 'NONE', #12059 ) ;
#1744 =( REPRESENTATION_RELATIONSHIP ('NONE','NONE', #12685, #13067 ) REPRESENTATION_RELATIONSHIP_WITH_TRANSFORMATION ( #14891 )SHAPE_REPRESENTATION_RELATIONSHIP( ) );
#1745 = CARTESIAN_POINT ( 'NONE',  ( 50.00050000000000239, 0.000000000000000000, 0.000000000000000000 ) ) ;
#1746 = DIRECTION ( 'NONE',  ( -1.000000000000000000, -0.000000000000000000, -0.000000000000000000 ) ) ;
#1747 = DIRECTION ( 'NONE',  ( 0.000000000000000000, 0.000000000000000000, 1.000000000000000000 ) ) ;
#1748 = DIRECTION ( 'NONE',  ( 0.000000000000000000, 0.000000000000000000, 1.000000000000000000 ) ) ;
#1749 = APPLICATION_PROTOCOL_DEFINITION ( 'draft international standard', 'automotive_design', 1998, #5486 ) ;
#1750 = CARTESIAN_POINT ( 'NONE',  ( 1.039999999999997593, 0.000000000000000000, 0.000000000000000000 ) ) ;
#1751 = ADVANCED_FACE ( 'NONE', ( #13452 ), #4577, .T. ) ;
#1752 = FACE_OUTER_BOUND ( 'NONE', #12919, .T. ) ;
#1753 = EDGE_LOOP ( 'NONE', ( #13832, #7384, #14688, #11419 ) ) ;
#1754 = CARTESIAN_POINT ( 'NONE',  ( -1.149999999999998135, 0.000000000000000000, 0.000000000000000000 ) ) ;
#1755 = CARTESIAN_POINT ( 'NONE',  ( -1.250000000000001110, 0.000000000000000000, 0.000000000000000000 ) ) ;
#1756 = CARTESIAN_POINT ( 'NONE',  ( 2.777260912398869852, 13.49730943211508816, -5.214906618940189809 ) ) ;
#1757 = VERTEX_POINT ( 'NONE', #1773 ) ;
#1758 = EDGE_CURVE ( 'NONE', #6683, #11986, #9775, .T. ) ;
#1759 = DIRECTION ( 'NONE',  ( 0.000000000000000000, 0.000000000000000000, 1.000000000000000000 ) ) ;
#1760 = CARTESIAN_POINT ( 'NONE',  ( -9.403944755730117677, -16.79473832354794993, 22.00000000000000000 ) ) ;
#1761 = EDGE_LOOP ( 'NONE', ( #3897, #12840, #9108, #15209, #13536, #5396, #5250, #11117 ) ) ;
#1762 = ORIENTED_EDGE ( 'NONE', *, *, #7585, .F. ) ;
#1763 =( NAMED_UNIT ( * ) PLANE_ANGLE_UNIT ( ) SI_UNIT ( $, .RADIAN. ) );
#1764 = CARTESIAN_POINT ( 'NONE',  ( 2.764680872515352661, 5.229914364928351489, 13.68080036884350292 ) ) ;
#1765 = DIRECTION ( 'NONE',  ( 0.000000000000000000, 0.000000000000000000, 1.000000000000000000 ) ) ;
#1766 = DIRECTION ( 'NONE',  ( 0.000000000000000000, 0.000000000000000000, 1.000000000000000000 ) ) ;
#1767 = CYLINDRICAL_SURFACE ( 'NONE', #9922, 28.06981291497571362 ) ;
#1768 = EDGE_CURVE ( 'NONE', #12657, #7299, #13123, .T. ) ;
#1769 = EDGE_CURVE ( 'NONE', #13658, #11133, #8990, .T. ) ;
#1770 = AXIS2_PLACEMENT_3D ( 'NONE', #1052, #6044, #3580 ) ;
#1771 = DIRECTION ( 'NONE',  ( 0.9148936170212769170, 0.4036950204470262649, -0.000000000000000000 ) ) ;
#1772 = VERTEX_POINT ( 'NONE', #5624 ) ;
#1773 = CARTESIAN_POINT ( 'NONE',  ( 19.25177984293775069, 7.759396820770414926, 7.000000000000000000 ) ) ;
#1774 = PLANE ( 'NONE',  #6975 ) ;
#1775 = SURFACE_STYLE_USAGE ( .BOTH. , #381 ) ;
#1776 = CIRCLE ( 'NONE', #6200, 5.999999999999999112 ) ;
#1777 = ORIENTED_EDGE ( 'NONE', *, *, #7772, .F. ) ;
#1778 = VERTEX_POINT ( 'NONE', #12531 ) ;
#1779 = VERTEX_POINT ( 'NONE', #997 ) ;
#1780 = ADVANCED_FACE ( 'NONE', ( #844 ), #2361, .T. ) ;
#1781 = DIRECTION ( 'NONE',  ( 1.000000000000000000, 0.000000000000000000, 0.000000000000000000 ) ) ;
#1782 = EDGE_CURVE ( 'NONE', #1577, #10971, #9148, .T. ) ;
#1783 = CARTESIAN_POINT ( 'NONE',  ( 2.790000000000000036, -20.65025570340076655, -12.51972505885016140 ) ) ;
#1784 = EDGE_CURVE ( 'NONE', #2017, #6698, #6767, .T. ) ;
#1785 = PRODUCT_DEFINITION_CONTEXT ( 'detailed design', #3121, 'design' ) ;
#1786 = DIRECTION ( 'NONE',  ( 0.9863939238321437486, 0.1643989873053572359, -0.000000000000000000 ) ) ;
#1787 = DIRECTION ( 'NONE',  ( 0.02857142857142857401, 0.9995917534020515305, -0.000000000000000000 ) ) ;
#1788 = EDGE_LOOP ( 'NONE', ( #2878, #682, #5226, #13096 ) ) ;
#1789 = CARTESIAN_POINT ( 'NONE',  ( 0.9999999999999997780, -6.008326913195983998, 0.000000000000000000 ) ) ;
#1790 = CARTESIAN_POINT ( 'NONE',  ( 0.000000000000000000, -23.48180575137736170, 5.535312321042622052 ) ) ;
#1791 = EDGE_CURVE ( 'NONE', #4429, #1582, #9724, .T. ) ;
#1792 = DIRECTION ( 'NONE',  ( 0.000000000000000000, 0.000000000000000000, 1.000000000000000000 ) ) ;
#1793 = DIRECTION ( 'NONE',  ( -1.000000000000000000, -0.000000000000000000, -0.000000000000000000 ) ) ;
#1794 = CARTESIAN_POINT ( 'NONE',  ( 2.789999999999999147, 0.000000000000000000, 0.000000000000000000 ) ) ;
#1795 = EDGE_LOOP ( 'NONE', ( #14098, #13831, #14406, #12541, #7881, #1799, #7159, #1308 ) ) ;
#1796 = CARTESIAN_POINT ( 'NONE',  ( 0.07473581742173279752, 14.31752701692944285, -5.299647274066949798 ) ) ;
#1797 = CARTESIAN_POINT ( 'NONE',  ( 0.007327513813773455648, 13.44898112152234937, 5.204526028255736847 ) ) ;
#1798 = ORIENTED_EDGE ( 'NONE', *, *, #5583, .T. ) ;
#1799 = ORIENTED_EDGE ( 'NONE', *, *, #7638, .T. ) ;
#1800 = CARTESIAN_POINT ( 'NONE',  ( -9.999999999999992895, -25.00000000000000000, -131.1575142076926852 ) ) ;
#1801 = DIRECTION ( 'NONE',  ( 0.000000000000000000, 0.000000000000000000, 1.000000000000000000 ) ) ;
#1802 =( NAMED_UNIT ( * ) SI_UNIT ( $, .STERADIAN. ) SOLID_ANGLE_UNIT ( ) );
#1803 = DIRECTION ( 'NONE',  ( 0.000000000000000000, 0.000000000000000000, 1.000000000000000000 ) ) ;
#1804 = CARTESIAN_POINT ( 'NONE',  ( 2.790000000000009361, -2.096460570596073936, -14.05347802000171065 ) ) ;
#1805 = VERTEX_POINT ( 'NONE', #5475 ) ;
#1806 = CARTESIAN_POINT ( 'NONE',  ( -5.209999999999999964, 0.000000000000000000, 0.000000000000000000 ) ) ;
#1807 = CARTESIAN_POINT ( 'NONE',  ( 75.20570977803312473, 12.97982004111159959, 4.000000000000000000 ) ) ;
#1808 = ORIENTED_EDGE ( 'NONE', *, *, #6015, .T. ) ;
#1809 = ADVANCED_FACE ( 'NONE', ( #3165 ), #13829, .T. ) ;
#1810 = CARTESIAN_POINT ( 'NONE',  ( 0.1713913650100259145, 0.000000000000000000, 4.424999999999999822 ) ) ;
#1811 = ORIENTED_EDGE ( 'NONE', *, *, #7772, .T. ) ;
#1812 = ORIENTED_EDGE ( 'NONE', *, *, #14545, .F. ) ;
#1813 = VERTEX_POINT ( 'NONE', #7767 ) ;
#1814 = CARTESIAN_POINT ( 'NONE',  ( 0.007327532539344137376, 2.217238903388563109, 14.24942254254690255 ) ) ;
#1815 = CYLINDRICAL_SURFACE ( 'NONE', #4126, 0.5999999999999999778 ) ;
#1816 = EDGE_CURVE ( 'NONE', #10954, #10191, #12750, .T. ) ;
#1817 = CIRCLE ( 'NONE', #8933, 4.000000000000000000 ) ;
#1818 = LINE ( 'NONE', #8729, #2381 ) ;
#1819 = AXIS2_PLACEMENT_3D ( 'NONE', #3638, #8391, #13159 ) ;
#1820 = CARTESIAN_POINT ( 'NONE',  ( 2.601776091974071115, -5.251266773802197640, -25.40949241676359094 ) ) ;
#1821 = PRODUCT_CONTEXT ( 'NONE', #10769, 'mechanical' ) ;
#1822 = CYLINDRICAL_SURFACE ( 'NONE', #7593, 2.524999999999995914 ) ;
#1823 = AXIS2_PLACEMENT_3D ( 'NONE', #2979, #11196, #671 ) ;
#1824 = FACE_OUTER_BOUND ( 'NONE', #11913, .T. ) ;
#1825 = CARTESIAN_POINT ( 'NONE',  ( 1.749999999999999778, 17.29145405592695539, -4.835383649608290924 ) ) ;
#1826 = VERTEX_POINT ( 'NONE', #3304 ) ;
#1827 = DIRECTION ( 'NONE',  ( 0.000000000000000000, 0.000000000000000000, 1.000000000000000000 ) ) ;
#1828 = DIRECTION ( 'NONE',  ( -0.000000000000000000, -0.000000000000000000, -1.000000000000000000 ) ) ;
#1829 = AXIS2_PLACEMENT_3D ( 'NONE', #7372, #8421, #13107 ) ;
#1830 = DIRECTION ( 'NONE',  ( 1.000000000000000000, 0.000000000000000000, 0.000000000000000000 ) ) ;
#1831 = ORIENTED_EDGE ( 'NONE', *, *, #2240, .T. ) ;
#1832 = AXIS2_PLACEMENT_3D ( 'NONE', #5697, #10372, #5476 ) ;
#1833 = APPLICATION_CONTEXT ( 'automotive_design' ) ;
#1834 = CARTESIAN_POINT ( 'NONE',  ( -16.64001273322991281, -7.794738323547949932, 14.99999999999999822 ) ) ;
#1835 = CARTESIAN_POINT ( 'NONE',  ( 0.02436607992776411782, 22.71065055754465689, -9.836394144775473691 ) ) ;
#1836 = ORIENTED_EDGE ( 'NONE', *, *, #9897, .T. ) ;
#1837 = ORIENTED_EDGE ( 'NONE', *, *, #14433, .F. ) ;
#1838 = CARTESIAN_POINT ( 'NONE',  ( 2.790000000000000036, 24.22479935914659777, -2.133490293297098273 ) ) ;
#1839 = DIRECTION ( 'NONE',  ( 0.000000000000000000, 0.000000000000000000, 1.000000000000000000 ) ) ;
#1840 = EDGE_CURVE ( 'NONE', #3303, #4132, #9475, .T. ) ;
#1841 = CARTESIAN_POINT ( 'NONE',  ( 0.006931054464085153848, 2.248820353273311756, -24.42321038836780644 ) ) ;
#1842 = CARTESIAN_POINT ( 'NONE',  ( 0.000000000000000000, -13.40591150984221080, -7.739906618939849103 ) ) ;
#1843 = CARTESIAN_POINT ( 'NONE',  ( 0.1085714285714285687, -3.798448662927795372, -0.8000000000000000444 ) ) ;
#1844 = CIRCLE ( 'NONE', #13857, 2.524999999999995914 ) ;
#1845 = AXIS2_PLACEMENT_3D ( 'NONE', #5193, #14783, #8928 ) ;
#1846 = EDGE_CURVE ( 'NONE', #3700, #6635, #6624, .T. ) ;
#1847 = CARTESIAN_POINT ( 'NONE',  ( 1.749999999999998002, 0.000000000000000000, 0.000000000000000000 ) ) ;
#1848 = CARTESIAN_POINT ( 'NONE',  ( 2.789999999999999147, 5.535312321043049266, -23.48180575137724446 ) ) ;
#1849 = VERTEX_POINT ( 'NONE', #3083 ) ;
#1850 = DIRECTION ( 'NONE',  ( -1.000000000000000000, -0.000000000000000000, -0.000000000000000000 ) ) ;
#1851 = CYLINDRICAL_SURFACE ( 'NONE', #15082, 2.999999999999988898 ) ;
#1852 = ORIENTED_EDGE ( 'NONE', *, *, #2015, .F. ) ;
#1853 = VECTOR ( 'NONE', #11773, 1000.000000000000000 ) ;
#1854 = EDGE_CURVE ( 'NONE', #11686, #6526, #3965, .T. ) ;
#1855 =( NAMED_UNIT ( * ) SI_UNIT ( $, .STERADIAN. ) SOLID_ANGLE_UNIT ( ) );
#1856 = AXIS2_PLACEMENT_3D ( 'NONE', #6396, #6233, #3013 ) ;
#1857 = EDGE_CURVE ( 'NONE', #3154, #6372, #5972, .T. ) ;
#1858 = VECTOR ( 'NONE', #2108, 1000.000000000000000 ) ;
#1859 = ORIENTED_EDGE ( 'NONE', *, *, #3148, .T. ) ;
#1860 = VERTEX_POINT ( 'NONE', #11521 ) ;
#1861 = VERTEX_POINT ( 'NONE', #15066 ) ;
#1862 = CARTESIAN_POINT ( 'NONE',  ( -14.40394475573011945, -10.79473832354794460, 12.00000000000000000 ) ) ;
#1863 = DIRECTION ( 'NONE',  ( -1.000000000000000000, 0.000000000000000000, 0.000000000000000000 ) ) ;
#1864 = CARTESIAN_POINT ( 'NONE',  ( -10.00000000000000000, 0.000000000000000000, 0.000000000000000000 ) ) ;
#1865 = CYLINDRICAL_SURFACE ( 'NONE', #10935, 2.999999999999988898 ) ;
#1866 = VECTOR ( 'NONE', #7703, 1000.000000000000000 ) ;
#1867 = ORIENTED_EDGE ( 'NONE', *, *, #8472, .T. ) ;
#1868 = CARTESIAN_POINT ( 'NONE',  ( -18.40394475573011945, -10.79473832354794460, -3.406384528788088688E-15 ) ) ;
#1869 = CARTESIAN_POINT ( 'NONE',  ( -10.00000000000000000, 0.000000000000000000, 0.000000000000000000 ) ) ;
#1870 = ADVANCED_FACE ( 'NONE', ( #4540 ), #2857, .T. ) ;
#1871 = CARTESIAN_POINT ( 'NONE',  ( 0.4286645550874384480, 15.76776810790841310, 5.200734291367693274 ) ) ;
#1872 = LINE ( 'NONE', #4418, #7681 ) ;
#1873 = EDGE_CURVE ( 'NONE', #3107, #988, #9246, .T. ) ;
#1874 = AXIS2_PLACEMENT_3D ( 'NONE', #1369, #10753, #11665 ) ;
#1875 = ORIENTED_EDGE ( 'NONE', *, *, #1681, .F. ) ;
#1876 = PLANE ( 'NONE',  #1389 ) ;
#1877 = AXIS2_PLACEMENT_3D ( 'NONE', #12439, #902, #10287 ) ;
#1878 = LINE ( 'NONE', #14642, #10434 ) ;
#1879 = ORIENTED_EDGE ( 'NONE', *, *, #987, .F. ) ;
#1880 = ORIENTED_EDGE ( 'NONE', *, *, #8495, .T. ) ;
#1881 = DIRECTION ( 'NONE',  ( 0.000000000000000000, 0.000000000000000000, 1.000000000000000000 ) ) ;
#1882 = ADVANCED_FACE ( 'NONE', ( #4312 ), #10075, .F. ) ;
#1883 =( LENGTH_UNIT ( ) NAMED_UNIT ( * ) SI_UNIT ( .MILLI., .METRE. ) );
#1884 = CARTESIAN_POINT ( 'NONE',  ( 1.749999999999998002, 20.02152543075374069, -19.67366047555509212 ) ) ;
#1885 = VERTEX_POINT ( 'NONE', #10148 ) ;
#1886 = VECTOR ( 'NONE', #7004, 1000.000000000000000 ) ;
#1887 = DIRECTION ( 'NONE',  ( -0.000000000000000000, -0.000000000000000000, -1.000000000000000000 ) ) ;
#1888 = AXIS2_PLACEMENT_3D ( 'NONE', #2323, #10170, #13712 ) ;
#1889 = EDGE_LOOP ( 'NONE', ( #1852, #6443, #10065, #13180, #5022, #10812 ) ) ;
#1890 = FACE_OUTER_BOUND ( 'NONE', #9487, .T. ) ;
#1891 = CARTESIAN_POINT ( 'NONE',  ( 2.789999999999999147, 2.680914349914567470E-13, -25.59481291497571220 ) ) ;
#1892 = VECTOR ( 'NONE', #10156, 1000.000000000000000 ) ;
#1893 = CIRCLE ( 'NONE', #10480, 17.95481323787947758 ) ;
#1894 = VERTEX_POINT ( 'NONE', #8991 ) ;
#1895 = CARTESIAN_POINT ( 'NONE',  ( 76.00000000000000000, 4.898587196589422689E-16, 5.500000000000005329 ) ) ;
#1896 = ORIENTED_EDGE ( 'NONE', *, *, #7500, .T. ) ;
#1897 = ORIENTED_EDGE ( 'NONE', *, *, #4607, .T. ) ;
#1898 = ORIENTED_EDGE ( 'NONE', *, *, #14445, .F. ) ;
#1899 = DIRECTION ( 'NONE',  ( 1.000000000000000000, 0.000000000000000000, 0.000000000000000000 ) ) ;
#1900 = VECTOR ( 'NONE', #3511, 1000.000000000000000 ) ;
#1901 = DIRECTION ( 'NONE',  ( 0.000000000000000000, 0.000000000000000000, 1.000000000000000000 ) ) ;
#1902 = CARTESIAN_POINT ( 'NONE',  ( 0.000000000000000000, 20.70663861606272249, 15.04425356660767932 ) ) ;
#1903 = PRODUCT_CONTEXT ( 'NONE', #13910, 'mechanical' ) ;
#1904 = AXIS2_PLACEMENT_3D ( 'NONE', #1144, #4834, #7284 ) ;
#1905 = CARTESIAN_POINT ( 'NONE',  ( 0.000000000000000000, 0.000000000000000000, 5.500000000000000000 ) ) ;
#1906 = VECTOR ( 'NONE', #8668, 1000.000000000000000 ) ;
#1907 = DIRECTION ( 'NONE',  ( 0.000000000000000000, 0.000000000000000000, 1.000000000000000000 ) ) ;
#1908 = DIRECTION ( 'NONE',  ( 0.000000000000000000, 0.000000000000000000, 1.000000000000000000 ) ) ;
#1909 = ORIENTED_EDGE ( 'NONE', *, *, #13404, .F. ) ;
#1910 = CARTESIAN_POINT ( 'NONE',  ( 0.02436607992776368414, 18.55949924794916228, -16.37294372382838148 ) ) ;
#1911 = DIRECTION ( 'NONE',  ( 0.000000000000000000, -0.3090169943749486170, 0.9510565162951530871 ) ) ;
#1912 = CARTESIAN_POINT ( 'NONE',  ( 0.000000000000000000, 0.000000000000000000, 10.00000000000000000 ) ) ;
#1913 = ORIENTED_EDGE ( 'NONE', *, *, #9541, .F. ) ;
#1914 = CIRCLE ( 'NONE', #14938, 0.1000000000000011297 ) ;
#1915 = STYLED_ITEM ( 'NONE', ( #6714 ), #15172 ) ;
#1916 = EDGE_CURVE ( 'NONE', #9387, #10729, #2530, .T. ) ;
#1917 = DIRECTION ( 'NONE',  ( 0.000000000000000000, 0.000000000000000000, 1.000000000000000000 ) ) ;
#1919 = TOROIDAL_SURFACE ( 'NONE', #3876, 24.12539914357697413, 8.000000000000000000 ) ;
#1918 = FACE_OUTER_BOUND ( 'NONE', #12715, .T. ) ;
#1920 = ORIENTED_EDGE ( 'NONE', *, *, #180, .F. ) ;
#1921 = AXIS2_PLACEMENT_3D ( 'NONE', #4330, #13703, #3182 ) ;
#1922 = VERTEX_POINT ( 'NONE', #10671 ) ;
#1923 = CYLINDRICAL_SURFACE ( 'NONE', #409, 6.000000000000001776 ) ;
#1924 = DIRECTION ( 'NONE',  ( -1.000000000000000000, -0.000000000000000000, -0.000000000000000000 ) ) ;
#1925 = DIRECTION ( 'NONE',  ( 0.000000000000000000, 0.000000000000000000, 1.000000000000000000 ) ) ;
#1926 = FACE_OUTER_BOUND ( 'NONE', #4356, .T. ) ;
#1927 = FACE_OUTER_BOUND ( 'NONE', #9836, .T. ) ;
#1928 = CIRCLE ( 'NONE', #4390, 4.000000000000000000 ) ;
#1929 = DIRECTION ( 'NONE',  ( -1.000000000000000000, 0.000000000000000000, 0.000000000000000000 ) ) ;
#1930 = DIRECTION ( 'NONE',  ( -0.9988110320138940956, -0.04874958797097371510, 0.000000000000000000 ) ) ;
#1931 = EDGE_CURVE ( 'NONE', #12415, #7949, #2462, .T. ) ;
#1932 = VERTEX_POINT ( 'NONE', #2604 ) ;
#1933 = CARTESIAN_POINT ( 'NONE',  ( 8.000000000000000000, 0.000000000000000000, 0.000000000000000000 ) ) ;
#1934 = VECTOR ( 'NONE', #13923, 1000.000000000000000 ) ;
#1935 = TOROIDAL_SURFACE ( 'NONE', #13710, 24.12539914357697413, 8.000000000000000000 ) ;
#1936 = LINE ( 'NONE', #4397, #846 ) ;
#1937 = ADVANCED_FACE ( 'NONE', ( #14133 ), #13407, .T. ) ;
#1938 = ORIENTED_EDGE ( 'NONE', *, *, #3558, .T. ) ;
#1939 = EDGE_CURVE ( 'NONE', #929, #11100, #10710, .T. ) ;
#1940 = VERTEX_POINT ( 'NONE', #7066 ) ;
#1941 = ORIENTED_EDGE ( 'NONE', *, *, #12061, .F. ) ;
#1942 = ORIENTED_EDGE ( 'NONE', *, *, #6245, .F. ) ;
#1943 = DIRECTION ( 'NONE',  ( -5.339417856040273846E-17, -1.063174570779084847E-17, 1.000000000000000000 ) ) ;
#1944 =( NAMED_UNIT ( * ) PLANE_ANGLE_UNIT ( ) SI_UNIT ( $, .RADIAN. ) );
#1945 = AXIS2_PLACEMENT_3D ( 'NONE', #10428, #416, #1664 ) ;
#1946 = AXIS2_PLACEMENT_3D ( 'NONE', #3215, #10121, #11276 ) ;
#1947 = CARTESIAN_POINT ( 'NONE',  ( 70.16198417812034904, 9.730076655429538590, 2.999999999999999112 ) ) ;
#1948 = CARTESIAN_POINT ( 'NONE',  ( 1.039999999999996705, -20.02152543075359503, 19.67366047555523423 ) ) ;
#1949 = ADVANCED_FACE ( 'NONE', ( #3680, #12971 ), #125, .T. ) ;
#1950 = ORIENTED_EDGE ( 'NONE', *, *, #14469, .T. ) ;
#1951 = DIRECTION ( 'NONE',  ( -0.000000000000000000, 0.000000000000000000, -1.000000000000000000 ) ) ;
#1952 = CARTESIAN_POINT ( 'NONE',  ( 2.789999999999999147, 7.739906618939895289, -13.40591150984218416 ) ) ;
#1953 = DIRECTION ( 'NONE',  ( 1.000000000000000000, 0.000000000000000000, 0.000000000000000000 ) ) ;
#1954 = VECTOR ( 'NONE', #13085, 999.9999999999998863 ) ;
#1955 = DIRECTION ( 'NONE',  ( 1.000000000000000000, -0.000000000000000000, -0.000000000000000000 ) ) ;
#1956 = ADVANCED_FACE ( 'NONE', ( #5922 ), #8208, .F. ) ;
#1957 = ORIENTED_EDGE ( 'NONE', *, *, #1648, .T. ) ;
#1958 = CARTESIAN_POINT ( 'NONE',  ( 0.02531912748605881155, 13.68080036884355621, -5.229914364928207604 ) ) ;
#1959 = DIRECTION ( 'NONE',  ( 0.000000000000000000, 0.000000000000000000, 1.000000000000000000 ) ) ;
#1960 = ORIENTED_EDGE ( 'NONE', *, *, #1370, .F. ) ;
#1961 = ORIENTED_EDGE ( 'NONE', *, *, #14379, .T. ) ;
#1962 = B_SPLINE_CURVE_WITH_KNOTS ( 'NONE', 3,
 ( #10367, #4391, #918, #5621, #2999, #4464 ),
 .UNSPECIFIED., .F., .F.,
 ( 4, 2, 4 ),
 ( 2.032124546189808531E-07, 0.001878594002992309232, 0.003756984793529999193 ),
 .UNSPECIFIED. ) ;
#1963 = CARTESIAN_POINT ( 'NONE',  ( 1.394999999999999574, -4.633866840649122132, 27.68468304288257542 ) ) ;
#1964 = EDGE_CURVE ( 'NONE', #4081, #10279, #8485, .T. ) ;
#1965 = CARTESIAN_POINT ( 'NONE',  ( 8.000000000000000000, 0.000000000000000000, 0.000000000000000000 ) ) ;
#1966 = VECTOR ( 'NONE', #13841, 1000.000000000000000 ) ;
#1967 = EDGE_CURVE ( 'NONE', #8601, #9577, #139, .T. ) ;
#1968 = ADVANCED_FACE ( 'NONE', ( #14053 ), #6050, .T. ) ;
#1969 = ORIENTED_EDGE ( 'NONE', *, *, #5841, .F. ) ;
#1970 = DIRECTION ( 'NONE',  ( -1.000000000000000000, 0.000000000000000000, -0.000000000000000000 ) ) ;
#1971 = VERTEX_POINT ( 'NONE', #4765 ) ;
#1972 = DIRECTION ( 'NONE',  ( 1.000000000000000000, 0.000000000000000000, 0.000000000000000000 ) ) ;
#1973 = DIRECTION ( 'NONE',  ( 0.9021244663126475327, 0.4314758942051350465, -1.141265444721583757E-16 ) ) ;
#1974 = VERTEX_POINT ( 'NONE', #1294 ) ;
#1975 = DIRECTION ( 'NONE',  ( -5.480158469902919838E-17, -1.051478716308701618E-16, -1.000000000000000000 ) ) ;
#1976 = ORIENTED_EDGE ( 'NONE', *, *, #6296, .T. ) ;
#1977 = AXIS2_PLACEMENT_3D ( 'NONE', #2826, #14447, #13201 ) ;
#1978 = ORIENTED_EDGE ( 'NONE', *, *, #12875, .F. ) ;
#1979 = EDGE_CURVE ( 'NONE', #6140, #8705, #471, .T. ) ;
#1980 = CARTESIAN_POINT ( 'NONE',  ( 0.000000000000000000, 0.4273491293402468805, 0.000000000000000000 ) ) ;
#1981 = ADVANCED_FACE ( 'NONE', ( #5985 ), #3522, .F. ) ;
#1982 = LINE ( 'NONE', #11413, #7043 ) ;
#1983 = CARTESIAN_POINT ( 'NONE',  ( 2.789999999999999147, 19.91106274590533687, -14.18181402625721077 ) ) ;
#1984 = APPLICATION_PROTOCOL_DEFINITION ( 'draft international standard', 'automotive_design', 1998, #6642 ) ;
#1985 = CARTESIAN_POINT ( 'NONE',  ( 0.07473575470096431583, -9.749517823374088010, 11.74839219818084324 ) ) ;
#1986 = EDGE_CURVE ( 'NONE', #9176, #13761, #14232, .T. ) ;
#1987 = DIRECTION ( 'NONE',  ( -0.000000000000000000, -0.000000000000000000, 1.000000000000000000 ) ) ;
#1988 = EDGE_LOOP ( 'NONE', ( #3045, #4241, #1408, #4625 ) ) ;
#1989 = FACE_OUTER_BOUND ( 'NONE', #55, .T. ) ;
#1990 = DIRECTION ( 'NONE',  ( 0.000000000000000000, 0.000000000000000000, 1.000000000000000000 ) ) ;
#1991 = CYLINDRICAL_SURFACE ( 'NONE', #10235, 2.524999999999995914 ) ;
#1992 = ADVANCED_FACE ( 'NONE', ( #8139 ), #6987, .F. ) ;
#1993 = VERTEX_POINT ( 'NONE', #9369 ) ;
#1994 = DIRECTION ( 'NONE',  ( 1.000000000000000000, 0.000000000000000000, 0.000000000000000000 ) ) ;
#1995 = CARTESIAN_POINT ( 'NONE',  ( 2.783068961317272993, 12.53626894672858683, -21.08061549536601476 ) ) ;
#1996 = ORIENTED_EDGE ( 'NONE', *, *, #13788, .F. ) ;
#1997 = VERTEX_POINT ( 'NONE', #2689 ) ;
#1998 = FACE_OUTER_BOUND ( 'NONE', #11226, .T. ) ;
#1999 = CARTESIAN_POINT ( 'NONE',  ( 2.790000000000060876, -5.211197193340600720, -13.21862218141521339 ) ) ;
#2000 = ORIENTED_EDGE ( 'NONE', *, *, #3343, .T. ) ;
#2001 = CARTESIAN_POINT ( 'NONE',  ( 101.6227766016837819, 5.204170427930421283E-15, -131.1575142076926852 ) ) ;
#2002 = FACE_OUTER_BOUND ( 'NONE', #150, .T. ) ;
#2003 = LINE ( 'NONE', #6686, #9194 ) ;
#2004 = DIRECTION ( 'NONE',  ( 0.000000000000000000, 0.000000000000000000, 1.000000000000000000 ) ) ;
#2005 = ORIENTED_EDGE ( 'NONE', *, *, #11028, .F. ) ;
#2006 = CARTESIAN_POINT ( 'NONE',  ( 67.23404255319145761, 28.93147646537026318, -130.1575142076926852 ) ) ;
#2007 = DIRECTION ( 'NONE',  ( 1.000000000000000000, 0.000000000000000000, 0.000000000000000000 ) ) ;
#2008 = VERTEX_POINT ( 'NONE', #9753 ) ;
#2009 = B_SPLINE_CURVE_WITH_KNOTS ( 'NONE', 3,
 ( #6961, #4674, #9408, #14105 ),
 .UNSPECIFIED., .F., .F.,
 ( 4, 4 ),
 ( 0.005258139959819248602, 0.005948405594583415848 ),
 .UNSPECIFIED. ) ;
#2010 = ORIENTED_EDGE ( 'NONE', *, *, #14740, .T. ) ;
#2011 = EDGE_LOOP ( 'NONE', ( #1942, #5259, #13694, #8912 ) ) ;
#2012 = ORIENTED_EDGE ( 'NONE', *, *, #987, .T. ) ;
#2013 = CARTESIAN_POINT ( 'NONE',  ( 1.039999999999997593, 0.000000000000000000, 0.000000000000000000 ) ) ;
#2014 = CARTESIAN_POINT ( 'NONE',  ( 0.7589665089996491254, -24.80232951178369660, -12.05173163741749320 ) ) ;
#2015 = EDGE_CURVE ( 'NONE', #446, #4654, #8716, .T. ) ;
#2016 = CARTESIAN_POINT ( 'NONE',  ( 2.031033467310410234, -12.98167595241039329, 24.32849926382746020 ) ) ;
#2017 = VERTEX_POINT ( 'NONE', #8661 ) ;
#2018 = CARTESIAN_POINT ( 'NONE',  ( 1.387778780781445676E-14, 0.000000000000000000, -7.000000000000007994 ) ) ;
#2019 = CARTESIAN_POINT ( 'NONE',  ( 8.961831343790189308, 9.104486995144789319, 4.000000000000003553 ) ) ;
#2020 = LINE ( 'NONE', #13546, #4525 ) ;
#2021 = AXIS2_PLACEMENT_3D ( 'NONE', #8124, #6895, #4908 ) ;
#2022 = DIRECTION ( 'NONE',  ( 0.000000000000000000, 0.000000000000000000, -1.000000000000000000 ) ) ;
#2023 = ORIENTED_EDGE ( 'NONE', *, *, #1183, .F. ) ;
#2024 = CARTESIAN_POINT ( 'NONE',  ( 0.5279273746168626769, -4.996265754456183927, -26.57710921259766224 ) ) ;
#2025 = CARTESIAN_POINT ( 'NONE',  ( 2.783025325906567371, -24.42374957165203853, -2.249040938978752013 ) ) ;
#2026 = ORIENTED_EDGE ( 'NONE', *, *, #4399, .F. ) ;
#2027 = ORIENTED_EDGE ( 'NONE', *, *, #9884, .T. ) ;
#2028 = CIRCLE ( 'NONE', #10620, 3.799999999999999378 ) ;
#2029 = SURFACE_STYLE_FILL_AREA ( #558 ) ;
#2030 = DIRECTION ( 'NONE',  ( -0.000000000000000000, -0.000000000000000000, 1.000000000000000000 ) ) ;
#2031 = EDGE_LOOP ( 'NONE', ( #7108, #9185, #13828, #4457 ) ) ;
#2032 = EDGE_CURVE ( 'NONE', #5828, #10832, #1525, .T. ) ;
#2033 = DIRECTION ( 'NONE',  ( 1.000000000000000000, 0.000000000000000000, 0.000000000000000000 ) ) ;
#2034 = APPLICATION_CONTEXT ( 'automotive_design' ) ;
#2035 = ORIENTED_EDGE ( 'NONE', *, *, #8689, .F. ) ;
#2036 = DIRECTION ( 'NONE',  ( 0.000000000000000000, -1.000000000000000000, -4.122115190439943875E-15 ) ) ;
#2037 = VERTEX_POINT ( 'NONE', #12116 ) ;
#2038 = FACE_OUTER_BOUND ( 'NONE', #14776, .T. ) ;
#2039 = FACE_OUTER_BOUND ( 'NONE', #8512, .T. ) ;
#2040 = ORIENTED_EDGE ( 'NONE', *, *, #3738, .F. ) ;
#2041 = EDGE_CURVE ( 'NONE', #1528, #2696, #6707, .T. ) ;
#2042 = EDGE_CURVE ( 'NONE', #4474, #8109, #10464, .T. ) ;
#2043 = VERTEX_POINT ( 'NONE', #1684 ) ;
#2044 = DIRECTION ( 'NONE',  ( -0.000000000000000000, -0.000000000000000000, 1.000000000000000000 ) ) ;
#2045 = DIRECTION ( 'NONE',  ( 0.000000000000000000, 0.000000000000000000, 1.000000000000000000 ) ) ;
#2046 = LINE ( 'NONE', #14745, #1646 ) ;
#2047 = CARTESIAN_POINT ( 'NONE',  ( 0.8956445960621760571, 24.59653223688280121, 12.96989951879416125 ) ) ;
#2048 = CONTEXT_DEPENDENT_SHAPE_REPRESENTATION ( #11458, #126 ) ;
#2049 = CARTESIAN_POINT ( 'NONE',  ( 2.789999999999999147, -22.71065055754445439, -9.836394144775947979 ) ) ;
#2050 = CARTESIAN_POINT ( 'NONE',  ( 0.07186814640506890284, 21.92302674874982316, -12.74240566898960303 ) ) ;
#2051 = VERTEX_POINT ( 'NONE', #8820 ) ;
#2052 = CARTESIAN_POINT ( 'NONE',  ( 61.98919079003883326, 3.953582723775848962, 4.000000000000000000 ) ) ;
#2053 = DIRECTION ( 'NONE',  ( -0.000000000000000000, -0.000000000000000000, -1.000000000000000000 ) ) ;
#2054 = EDGE_CURVE ( 'NONE', #3198, #8635, #12421, .T. ) ;
#2055 = CARTESIAN_POINT ( 'NONE',  ( 2.764680872513935128, -5.229914364928447412, 13.68080036884346917 ) ) ;
#2056 = ADVANCED_FACE ( 'NONE', ( #13435 ), #8595, .T. ) ;
#2057 = PRODUCT_DEFINITION_FORMATION_WITH_SPECIFIED_SOURCE ( 'ANY', '', #2480, .NOT_KNOWN. ) ;
#2058 = ORIENTED_EDGE ( 'NONE', *, *, #12577, .T. ) ;
#2059 = EDGE_CURVE ( 'NONE', #12893, #11975, #10007, .T. ) ;
#2060 = DIRECTION ( 'NONE',  ( 0.000000000000000000, 0.000000000000000000, 1.000000000000000000 ) ) ;
#2061 = DIRECTION ( 'NONE',  ( -1.000000000000000000, 0.000000000000000000, -0.000000000000000000 ) ) ;
#2062 = ORIENTED_EDGE ( 'NONE', *, *, #1527, .F. ) ;
#2063 = VERTEX_POINT ( 'NONE', #2830 ) ;
#2064 = CARTESIAN_POINT ( 'NONE',  ( 2.789999999999999147, 0.000000000000000000, 0.000000000000000000 ) ) ;
#2065 = LINE ( 'NONE', #6682, #14927 ) ;
#2066 = EDGE_LOOP ( 'NONE', ( #2156, #3607, #7181, #7620, #5886, #1396, #303, #3086, #8875, #8957, #1193, #6098, #2265, #14266, #3257, #5444 ) ) ;
#2067 = CARTESIAN_POINT ( 'NONE',  ( 2.789999999999999147, 23.48180575137737947, -5.535312321042476391 ) ) ;
#2068 = CARTESIAN_POINT ( 'NONE',  ( 1.749999999999998002, 0.000000000000000000, 0.000000000000000000 ) ) ;
#2069 = SURFACE_STYLE_FILL_AREA ( #12592 ) ;
#2070 = EDGE_CURVE ( 'NONE', #12014, #3521, #14593, .T. ) ;
#2071 = CARTESIAN_POINT ( 'NONE',  ( 0.000000000000000000, 0.000000000000000000, 3.895000000000000462 ) ) ;
#2072 = CARTESIAN_POINT ( 'NONE',  ( 18.21994936526786901, -20.29667510578869027, 4.000000000000000000 ) ) ;
#2073 = AXIS2_PLACEMENT_3D ( 'NONE', #7314, #294, #1239 ) ;
#2074 = ORIENTED_EDGE ( 'NONE', *, *, #9768, .F. ) ;
#2075 = CARTESIAN_POINT ( 'NONE',  ( 1.749999999999999778, 17.39253030560841395, 4.458161950358562109 ) ) ;
#2076 = VECTOR ( 'NONE', #8244, 1000.000000000000000 ) ;
#2077 = LINE ( 'NONE', #13912, #5028 ) ;
#2078 = VERTEX_POINT ( 'NONE', #9893 ) ;
#2079 = DIRECTION ( 'NONE',  ( 1.000000000000000000, 0.000000000000000000, 0.000000000000000000 ) ) ;
#2080 = ORIENTED_EDGE ( 'NONE', *, *, #12668, .T. ) ;
#2081 = EDGE_LOOP ( 'NONE', ( #12736, #9559, #6883, #9632 ) ) ;
#2082 = VERTEX_POINT ( 'NONE', #14368 ) ;
#2083 = FACE_OUTER_BOUND ( 'NONE', #4286, .T. ) ;
#2084 = AXIS2_PLACEMENT_3D ( 'NONE', #4593, #2122, #6813 ) ;
#2085 = VECTOR ( 'NONE', #3110, 1000.000000000000000 ) ;
#2086 = FACE_OUTER_BOUND ( 'NONE', #13410, .T. ) ;
#2087 = CARTESIAN_POINT ( 'NONE',  ( 0.000000000000000000, 0.000000000000000000, 0.000000000000000000 ) ) ;
#2088 = ORIENTED_EDGE ( 'NONE', *, *, #3845, .T. ) ;
#2090 = CARTESIAN_POINT ( 'NONE',  ( 2.789999999999999147, -25.59481291497571220, -1.787276233276378314E-13 ) ) ;
#2089 = PRODUCT_DEFINITION_FORMATION_WITH_SPECIFIED_SOURCE ( 'ANY', '', #9463, .NOT_KNOWN. ) ;
#2091 = DIRECTION ( 'NONE',  ( -1.000000000000000000, 0.000000000000000000, 0.000000000000000000 ) ) ;
#2092 = AXIS2_PLACEMENT_3D ( 'NONE', #9331, #4571, #9393 ) ;
#2093 = VECTOR ( 'NONE', #10847, 1000.000000000000000 ) ;
#2094 = CARTESIAN_POINT ( 'NONE',  ( 2.765633920072236407, 2.336989772644613161, -24.63872515616080250 ) ) ;
#2095 = EDGE_LOOP ( 'NONE', ( #8631, #14510 ) ) ;
#2096 = DIRECTION ( 'NONE',  ( 0.000000000000000000, 0.000000000000000000, 1.000000000000000000 ) ) ;
#2097 = CARTESIAN_POINT ( 'NONE',  ( 0.000000000000000000, -12.98979500319698488, 5.249430348645709010 ) ) ;
#2098 = ORIENTED_EDGE ( 'NONE', *, *, #9330, .T. ) ;
#2099 = VERTEX_POINT ( 'NONE', #7603 ) ;
#2100 = AXIS2_PLACEMENT_3D ( 'NONE', #4098, #12236, #6166 ) ;
#2101 = CIRCLE ( 'NONE', #8723, 4.000000000000000888 ) ;
#2102 = SURFACE_SIDE_STYLE ('',( #8863 ) ) ;
#2103 = CARTESIAN_POINT ( 'NONE',  ( 0.5279272933715191130, -18.56460150496952366, 19.66369668717026897 ) ) ;
#2104 = B_SPLINE_CURVE_WITH_KNOTS ( 'NONE', 3,
 ( #15134, #8562, #14496, #5751, #8129, #7053, #6972, #7419 ),
 .UNSPECIFIED., .F., .F.,
 ( 4, 2, 2, 4 ),
 ( 1.984117563342666817E-07, 0.001895214258086351218, 0.002842722181251362227, 0.003790230104416373452 ),
 .UNSPECIFIED. ) ;
#2105 = ORIENTED_EDGE ( 'NONE', *, *, #2898, .T. ) ;
#2106 = CARTESIAN_POINT ( 'NONE',  ( 2.782650442329440921, -11.23191127083869567, 9.045126717605739941 ) ) ;
#2107 = EDGE_CURVE ( 'NONE', #14957, #4472, #1137, .T. ) ;
#2108 = DIRECTION ( 'NONE',  ( -1.000000000000000000, -0.000000000000000000, 0.000000000000000000 ) ) ;
#2109 = CARTESIAN_POINT ( 'NONE',  ( 0.000000000000000000, 0.000000000000000000, 3.000000000000000000 ) ) ;
#2110 = EDGE_LOOP ( 'NONE', ( #7467, #6376, #974, #76 ) ) ;
#2111 = VECTOR ( 'NONE', #11579, 1000.000000000000000 ) ;
#2112 = CARTESIAN_POINT ( 'NONE',  ( 83.50748565343083385, 13.38500995229612478, 2.999999999999999112 ) ) ;
#2113 = ADVANCED_FACE ( 'NONE', ( #6290 ), #14525, .F. ) ;
#2114 = CARTESIAN_POINT ( 'NONE',  ( 0.000000000000000000, -15.04425356660744839, -20.70663861606288236 ) ) ;
#2115 = ORIENTED_EDGE ( 'NONE', *, *, #1223, .F. ) ;
#2116 = EDGE_CURVE ( 'NONE', #13784, #883, #8011, .T. ) ;
#2117 = ORIENTED_EDGE ( 'NONE', *, *, #1247, .F. ) ;
#2118 = DIRECTION ( 'NONE',  ( 0.9021244663126475327, 0.4314758942051350465, -1.141265444721583757E-16 ) ) ;
#2119 = DIRECTION ( 'NONE',  ( 0.000000000000000000, 0.000000000000000000, 1.000000000000000000 ) ) ;
#2120 = VECTOR ( 'NONE', #11371, 1000.000000000000000 ) ;
#2121 = DIRECTION ( 'NONE',  ( 0.000000000000000000, 0.000000000000000000, 1.000000000000000000 ) ) ;
#2122 = DIRECTION ( 'NONE',  ( -1.576560579138138762E-17, 1.359337748750801608E-17, -1.000000000000000000 ) ) ;
#2123 = ITEM_DEFINED_TRANSFORMATION ( 'NONE', 'NONE', #9444,  #1376 ) ;
#2124 = CARTESIAN_POINT ( 'NONE',  ( 2.789999999999999147, 7.909232158574813099, 24.34211360614303388 ) ) ;
#2125 = AXIS2_PLACEMENT_3D ( 'NONE', #5682, #15053, #13520 ) ;
#2126 =( GEOMETRIC_REPRESENTATION_CONTEXT ( 3 ) GLOBAL_UNCERTAINTY_ASSIGNED_CONTEXT ( ( #1634 ) ) GLOBAL_UNIT_ASSIGNED_CONTEXT ( ( #6541, #8765, #3857 ) ) REPRESENTATION_CONTEXT ( 'NONE', 'WORKASPACE' ) );
#2127 = CARTESIAN_POINT ( 'NONE',  ( 2.765633920072239071, -16.37294372382844543, -18.55949924794910544 ) ) ;
#2128 = AXIS2_PLACEMENT_3D ( 'NONE', #318, #3791, #5040 ) ;
#2129 = EDGE_CURVE ( 'NONE', #228, #7999, #1387, .T. ) ;
#2130 = ORIENTED_EDGE ( 'NONE', *, *, #840, .F. ) ;
#2131 = CARTESIAN_POINT ( 'NONE',  ( 2.697960337741387882, 2.583706482362242873, -15.03709480088669359 ) ) ;
#2132 = EDGE_CURVE ( 'NONE', #10310, #8382, #9978, .T. ) ;
#2133 = DIRECTION ( 'NONE',  ( -0.000000000000000000, -0.000000000000000000, 1.000000000000000000 ) ) ;
#2134 = LINE ( 'NONE', #13661, #3366 ) ;
#2135 = MECHANICAL_DESIGN_GEOMETRIC_PRESENTATION_REPRESENTATION (  '', ( #3118 ), #5350 ) ;
#2136 = ORIENTED_EDGE ( 'NONE', *, *, #7399, .T. ) ;
#2137 = DIRECTION ( 'NONE',  ( 0.000000000000000000, 0.000000000000000000, 1.000000000000000000 ) ) ;
#2138 = CARTESIAN_POINT ( 'NONE',  ( 2.765633920072234631, -21.30679549418640306, 12.59161484032904887 ) ) ;
#2139 = ORIENTED_EDGE ( 'NONE', *, *, #5417, .T. ) ;
#2140 = COLOUR_RGB ( '',0.8941176470588234615, 0.8941176470588234615, 0.8941176470588234615 ) ;
#2141 = ORIENTED_EDGE ( 'NONE', *, *, #980, .F. ) ;
#2142 = VECTOR ( 'NONE', #4991, 1000.000000000000114 ) ;
#2143 = CARTESIAN_POINT ( 'NONE',  ( 2.789999999999999147, 9.836394144776026138, -22.71065055754441531 ) ) ;
#2144 = DIRECTION ( 'NONE',  ( 0.000000000000000000, 0.000000000000000000, 1.000000000000000000 ) ) ;
#2145 = ORIENTED_EDGE ( 'NONE', *, *, #13176, .F. ) ;
#2146 = AXIS2_PLACEMENT_3D ( 'NONE', #12759, #9157, #2169 ) ;
#2147 = CARTESIAN_POINT ( 'NONE',  ( 2.597943646031691145, -15.58455734132168935, 2.883512197588957271 ) ) ;
#2148 = DIRECTION ( 'NONE',  ( 0.000000000000000000, 0.000000000000000000, 1.000000000000000000 ) ) ;
#2149 = DIRECTION ( 'NONE',  ( -1.000000000000000000, -0.000000000000000000, -0.000000000000000000 ) ) ;
#2150 = EDGE_CURVE ( 'NONE', #11004, #7400, #13908, .T. ) ;
#2151 = VECTOR ( 'NONE', #14804, 1000.000000000000000 ) ;
#2152 = DIRECTION ( 'NONE',  ( -5.480158469902919838E-17, -1.051478716308701618E-16, -1.000000000000000000 ) ) ;
#2153 = FACE_OUTER_BOUND ( 'NONE', #11801, .T. ) ;
#2154 = ADVANCED_FACE ( 'NONE', ( #586 ), #5306, .T. ) ;
#2155 = EDGE_CURVE ( 'NONE', #15073, #14161, #12432, .T. ) ;
#2156 = ORIENTED_EDGE ( 'NONE', *, *, #7988, .F. ) ;
#2157 = CARTESIAN_POINT ( 'NONE',  ( 2.582362678678089551, 15.57879356040263197, 2.899259574942802065 ) ) ;
#2158 = VECTOR ( 'NONE', #12105, 1000.000000000000000 ) ;
#2159 = AXIS2_PLACEMENT_3D ( 'NONE', #2430, #13082, #1426 ) ;
#2160 = FACE_OUTER_BOUND ( 'NONE', #10784, .T. ) ;
#2161 = CIRCLE ( 'NONE', #7069, 4.000000000000000000 ) ;
#2162 = EDGE_LOOP ( 'NONE', ( #6708, #1880, #6992, #3959 ) ) ;
#2163 = EDGE_CURVE ( 'NONE', #12183, #9373, #674, .T. ) ;
#2164 = SURFACE_STYLE_FILL_AREA ( #4316 ) ;
#2165 = ORIENTED_EDGE ( 'NONE', *, *, #6171, .T. ) ;
#2166 = EDGE_LOOP ( 'NONE', ( #14014, #1064, #11022, #7668, #9543, #14118 ) ) ;
#2167 = ORIENTED_EDGE ( 'NONE', *, *, #3111, .F. ) ;
#2168 = CARTESIAN_POINT ( 'NONE',  ( 2.601776105308174269, 25.78859396478527799, 2.857713464478781162 ) ) ;
#2169 = DIRECTION ( 'NONE',  ( 0.000000000000000000, 0.000000000000000000, 1.000000000000000000 ) ) ;
#2170 = AXIS2_PLACEMENT_3D ( 'NONE', #13922, #4406, #15077 ) ;
#2171 = CARTESIAN_POINT ( 'NONE',  ( 4.000000000000000888, 4.898587196589413815E-16, 10.00000000000000000 ) ) ;
#2172 = AXIS2_PLACEMENT_3D ( 'NONE', #13204, #5001, #5160 ) ;
#2173 = CARTESIAN_POINT ( 'NONE',  ( 18.87754531448929995, -24.24225080111726527, 7.000000000000000000 ) ) ;
#2174 = ORIENTED_EDGE ( 'NONE', *, *, #58, .F. ) ;
#2175 = DIRECTION ( 'NONE',  ( -0.9148936170212765839, -0.4036950204470271530, 0.000000000000000000 ) ) ;
#2176 = CARTESIAN_POINT ( 'NONE',  ( 1.394999999999999574, 4.458161950358503489, 17.39253030560843172 ) ) ;
#2177 = CARTESIAN_POINT ( 'NONE',  ( 0.5431871198829162362, 16.57708379306436441, -3.619024283482057847 ) ) ;
#2178 = ADVANCED_FACE ( 'NONE', ( #15050 ), #4288, .T. ) ;
#2179 = AXIS2_PLACEMENT_3D ( 'NONE', #10380, #2241, #6855 ) ;
#2180 = AXIS2_PLACEMENT_3D ( 'NONE', #13581, #14822, #3143 ) ;
#2181 = ORIENTED_EDGE ( 'NONE', *, *, #12438, .T. ) ;
#2182 = DIRECTION ( 'NONE',  ( 1.000000000000000000, 0.000000000000000000, 0.000000000000000000 ) ) ;
#2183 = DIRECTION ( 'NONE',  ( 0.8406209333187990573, 0.5416238976136774630, 0.000000000000000000 ) ) ;
#2184 = ORIENTED_EDGE ( 'NONE', *, *, #10571, .F. ) ;
#2185 = VERTEX_POINT ( 'NONE', #3361 ) ;
#2186 = DIRECTION ( 'NONE',  ( 1.000000000000000000, 0.000000000000000000, 0.000000000000000000 ) ) ;
#2187 = ORIENTED_EDGE ( 'NONE', *, *, #2481, .T. ) ;
#2188 = PLANE ( 'NONE',  #4532 ) ;
#2189 = DIRECTION ( 'NONE',  ( 0.000000000000000000, -0.8660254037844397068, 0.4999999999999980571 ) ) ;
#2190 = AXIS2_PLACEMENT_3D ( 'NONE', #15212, #11795, #5966 ) ;
#2191 = AXIS2_PLACEMENT_3D ( 'NONE', #1905, #6598, #10277 ) ;
#2192 = EDGE_CURVE ( 'NONE', #5464, #448, #820, .T. ) ;
#2193 = DIRECTION ( 'NONE',  ( 2.081668171172168513E-16, -1.000000000000000000, 0.000000000000000000 ) ) ;
#2194 = LINE ( 'NONE', #14091, #10899 ) ;
#2195 = VERTEX_POINT ( 'NONE', #3144 ) ;
#2196 = DIRECTION ( 'NONE',  ( 0.000000000000000000, 0.000000000000000000, -1.000000000000000000 ) ) ;
#2197 = CARTESIAN_POINT ( 'NONE',  ( -1.149999999999998135, 0.000000000000000000, 0.000000000000000000 ) ) ;
#2198 = ORIENTED_EDGE ( 'NONE', *, *, #7466, .T. ) ;
#2199 = B_SPLINE_CURVE_WITH_KNOTS ( 'NONE', 3,
 ( #8355, #4992, #13032, #2519, #3743, #9658 ),
 .UNSPECIFIED., .F., .F.,
 ( 4, 2, 4 ),
 ( 1.979325885420574018E-07, 0.001878588715165606469, 0.003756979497742670565 ),
 .UNSPECIFIED. ) ;
#2200 = EDGE_LOOP ( 'NONE', ( #5137, #8175 ) ) ;
#2201 = CARTESIAN_POINT ( 'NONE',  ( 1.039999999999998259, -12.83329210556822986, -12.55714665600000757 ) ) ;
#2202 = AXIS2_PLACEMENT_3D ( 'NONE', #692, #12593, #5402 ) ;
#2203 = FACE_OUTER_BOUND ( 'NONE', #11246, .T. ) ;
#2204 = EDGE_CURVE ( 'NONE', #4704, #4042, #8972, .T. ) ;
#2205 = CARTESIAN_POINT ( 'NONE',  ( 0.02436607992776541887, 12.59161484032942901, -21.30679549418617924 ) ) ;
#2206 = DIRECTION ( 'NONE',  ( 1.000000000000000000, 0.000000000000000000, 0.000000000000000000 ) ) ;
#2207 = CONTEXT_DEPENDENT_SHAPE_REPRESENTATION ( #2321, #8364 ) ;
#2208 = ADVANCED_FACE ( 'NONE', ( #13742 ), #5387, .T. ) ;
#2209 = DIRECTION ( 'NONE',  ( 1.000000000000000000, 0.000000000000000000, 0.000000000000000000 ) ) ;
#2210 = ORIENTED_EDGE ( 'NONE', *, *, #5514, .F. ) ;
#2211 = FACE_OUTER_BOUND ( 'NONE', #12320, .T. ) ;
#2212 = DIRECTION ( 'NONE',  ( -0.000000000000000000, -0.000000000000000000, -1.000000000000000000 ) ) ;
#2213 = DIRECTION ( 'NONE',  ( 0.000000000000000000, 0.000000000000000000, 1.000000000000000000 ) ) ;
#2214 = AXIS2_PLACEMENT_3D ( 'NONE', #3057, #670, #12646 ) ;
#2215 = DIRECTION ( 'NONE',  ( -1.000000000000000000, 0.000000000000000000, -0.000000000000000000 ) ) ;
#2216 = VERTEX_POINT ( 'NONE', #5606 ) ;
#2217 = FACE_OUTER_BOUND ( 'NONE', #7652, .T. ) ;
#2218 = CARTESIAN_POINT ( 'NONE',  ( 1.394999999999998685, 12.83329210556849276, -12.55714665599973756 ) ) ;
#2219 = ORIENTED_EDGE ( 'NONE', *, *, #4884, .F. ) ;
#2220 = VERTEX_POINT ( 'NONE', #12514 ) ;
#2221 = CARTESIAN_POINT ( 'NONE',  ( 1.039999999999997149, 17.39253030560841751, -4.458161950358562997 ) ) ;
#2222 = CARTESIAN_POINT ( 'NONE',  ( -1.250000000000001110, 0.000000000000000000, 0.000000000000000000 ) ) ;
#2223 = ORIENTED_EDGE ( 'NONE', *, *, #10206, .F. ) ;
#2224 = DIRECTION ( 'NONE',  ( -1.000000000000000000, -0.000000000000000000, -0.000000000000000000 ) ) ;
#2225 = CARTESIAN_POINT ( 'NONE',  ( 75.20570977803312473, 12.97982004111159959, 2.999999999999999112 ) ) ;
#2226 = CARTESIAN_POINT ( 'NONE',  ( 2.789999999999999147, 0.000000000000000000, 0.000000000000000000 ) ) ;
#2227 = DIRECTION ( 'NONE',  ( 0.000000000000000000, 0.000000000000000000, 1.000000000000000000 ) ) ;
#2228 = FACE_OUTER_BOUND ( 'NONE', #904, .T. ) ;
#2229 = ORIENTED_EDGE ( 'NONE', *, *, #2615, .T. ) ;
#2230 = DIRECTION ( 'NONE',  ( 0.000000000000000000, 0.000000000000000000, 1.000000000000000000 ) ) ;
#2231 = EDGE_CURVE ( 'NONE', #9019, #14061, #10282, .T. ) ;
#2232 = PRODUCT_DEFINITION_SHAPE ( 'NONE', 'NONE',  #15237 ) ;
#2233 = DIRECTION ( 'NONE',  ( 1.445602896647338917E-16, -1.000000000000000000, 0.000000000000000000 ) ) ;
#2234 = VERTEX_POINT ( 'NONE', #4371 ) ;
#2235 = PRESENTATION_STYLE_ASSIGNMENT (( #4242 ) ) ;
#2236 = ORIENTED_EDGE ( 'NONE', *, *, #15083, .T. ) ;
#2237 = ORIENTED_EDGE ( 'NONE', *, *, #14137, .T. ) ;
#2238 = EDGE_LOOP ( 'NONE', ( #13285, #3788, #14789, #4277 ) ) ;
#2239 = DIRECTION ( 'NONE',  ( 1.000000000000000000, 0.000000000000000000, 0.000000000000000000 ) ) ;
#2240 = EDGE_CURVE ( 'NONE', #4703, #11571, #13885, .T. ) ;
#2241 = DIRECTION ( 'NONE',  ( 0.000000000000000000, 0.000000000000000000, -1.000000000000000000 ) ) ;
#2242 = EDGE_CURVE ( 'NONE', #10729, #12348, #10059, .T. ) ;
#2243 = CARTESIAN_POINT ( 'NONE',  ( -19.40394475573012301, -7.794738323547950820, 16.99999999999999645 ) ) ;
#2244 = FACE_OUTER_BOUND ( 'NONE', #14397, .T. ) ;
#2245 = DIRECTION ( 'NONE',  ( 0.000000000000000000, 0.000000000000000000, 1.000000000000000000 ) ) ;
#2246 = VERTEX_POINT ( 'NONE', #6518 ) ;
#2247 = CARTESIAN_POINT ( 'NONE',  ( -14.40394475573011945, -4.794738323547946379, 22.00000000000000000 ) ) ;
#2248 = EDGE_CURVE ( 'NONE', #6366, #11582, #5471, .T. ) ;
#2249 = DIRECTION ( 'NONE',  ( 1.000000000000000000, 0.000000000000000000, 0.000000000000000000 ) ) ;
#2250 = ADVANCED_FACE ( 'NONE', ( #6674 ), #11281, .F. ) ;
#2251 = ORIENTED_EDGE ( 'NONE', *, *, #3001, .F. ) ;
#2252 = CARTESIAN_POINT ( 'NONE',  ( -14.40394475573011945, -10.79473832354794460, -5.000000000000000000 ) ) ;
#2253 = CARTESIAN_POINT ( 'NONE',  ( 80.00000000000000000, 0.000000000000000000, 4.500000000000000888 ) ) ;
#2254 = EDGE_CURVE ( 'NONE', #10930, #7241, #8915, .T. ) ;
#2255 = VERTEX_POINT ( 'NONE', #7968 ) ;
#2256 = EDGE_LOOP ( 'NONE', ( #4202, #12754, #1035, #5511 ) ) ;
#2257 = CYLINDRICAL_SURFACE ( 'NONE', #4821, 2.524999999999995914 ) ;
#2258 = EDGE_CURVE ( 'NONE', #14366, #3394, #7658, .T. ) ;
#2259 = ORIENTED_EDGE ( 'NONE', *, *, #2150, .F. ) ;
#2260 = VECTOR ( 'NONE', #7431, 1000.000000000000000 ) ;
#2261 = CARTESIAN_POINT ( 'NONE',  ( 2.764680872515354437, 13.68080036884355621, -5.229914364928207604 ) ) ;
#2262 = CARTESIAN_POINT ( 'NONE',  ( 2.790000000000008029, -11.12243880662619233, 8.842327429719055942 ) ) ;
#2263 = DIRECTION ( 'NONE',  ( 0.000000000000000000, 0.000000000000000000, 1.000000000000000000 ) ) ;
#2264 = FACE_OUTER_BOUND ( 'NONE', #3407, .T. ) ;
#2265 = ORIENTED_EDGE ( 'NONE', *, *, #2575, .T. ) ;
#2266 = DIRECTION ( 'NONE',  ( 0.000000000000000000, 0.000000000000000000, 1.000000000000000000 ) ) ;
#2267 = CARTESIAN_POINT ( 'NONE',  ( 2.601776121706764311, -19.18368891937477727, -17.47009390565512632 ) ) ;
#2268 = ORIENTED_EDGE ( 'NONE', *, *, #5962, .F. ) ;
#2269 = CIRCLE ( 'NONE', #12323, 0.5999999999999998668 ) ;
#2270 = VECTOR ( 'NONE', #14877, 1000.000000000000000 ) ;
#2271 = ORIENTED_EDGE ( 'NONE', *, *, #6899, .F. ) ;
#2272 = CARTESIAN_POINT ( 'NONE',  ( 0.000000000000000000, 20.62201879784911540, 12.52067188844362100 ) ) ;
#2273 = CARTESIAN_POINT ( 'NONE',  ( 1.039999999999998259, 12.52377138324223615, 25.12109765559657859 ) ) ;
#2274 = CARTESIAN_POINT ( 'NONE',  ( 2.765633920072238183, -5.391175441198789109, 24.15498966839961170 ) ) ;
#2275 = DIRECTION ( 'NONE',  ( -1.445602896647338917E-16, 1.000000000000000000, -0.000000000000000000 ) ) ;
#2276 = CONTEXT_DEPENDENT_SHAPE_REPRESENTATION ( #12241, #3696 ) ;
#2277 = CARTESIAN_POINT ( 'NONE',  ( 0.000000000000000000, 13.87420763704361448, -1.948757464274226470 ) ) ;
#2278 = CARTESIAN_POINT ( 'NONE',  ( 1.599999999999999867, -5.408326913195983465, 0.000000000000000000 ) ) ;
#2279 = ADVANCED_FACE ( 'NONE', ( #14982 ), #13582, .T. ) ;
#2280 = ORIENTED_EDGE ( 'NONE', *, *, #13596, .T. ) ;
#2282 = VECTOR ( 'NONE', #169, 1000.000000000000114 ) ;
#2281 = DIRECTION ( 'NONE',  ( -0.000000000000000000, -0.000000000000000000, -1.000000000000000000 ) ) ;
#2283 = LINE ( 'NONE', #14343, #4969 ) ;
#2284 = CARTESIAN_POINT ( 'NONE',  ( -14.40394475573012301, -16.79473832354794993, 16.99999999999999645 ) ) ;
#2285 = DIRECTION ( 'NONE',  ( 0.000000000000000000, 0.000000000000000000, 1.000000000000000000 ) ) ;
#2286 = ORIENTED_EDGE ( 'NONE', *, *, #14935, .F. ) ;
#2287 = EDGE_CURVE ( 'NONE', #2216, #1136, #10843, .T. ) ;
#2288 = DIRECTION ( 'NONE',  ( 1.000000000000000000, 0.000000000000000000, 0.000000000000000000 ) ) ;
#2289 = VERTEX_POINT ( 'NONE', #5677 ) ;
#2290 = DIRECTION ( 'NONE',  ( -1.000000000000000000, 0.000000000000000000, 0.000000000000000000 ) ) ;
#2291 = CARTESIAN_POINT ( 'NONE',  ( 2.790000000000076419, 2.133839912091138213, -24.22524813288759660 ) ) ;
#2292 = DIRECTION ( 'NONE',  ( -1.000000000000000000, -0.000000000000000000, -0.000000000000000000 ) ) ;
#2293 = CARTESIAN_POINT ( 'NONE',  ( 1.394999999999999574, 12.52377138324224148, 25.12109765559658570 ) ) ;
#2294 = CARTESIAN_POINT ( 'NONE',  ( -7.680503837993603605E-14, 23.69897269326676437, 5.456611084821939350 ) ) ;
#2295 = CARTESIAN_POINT ( 'NONE',  ( 0.1855656748306439008, -25.77772010606603814, -2.851997810081915663 ) ) ;
#2296 = CARTESIAN_POINT ( 'NONE',  ( 1.599999999999999867, -5.408326913195983465, -0.8000000000000000444 ) ) ;
#2297 = EDGE_LOOP ( 'NONE', ( #4906, #13957, #12309, #12977, #13907, #1270, #11727, #7776 ) ) ;
#2298 = DIRECTION ( 'NONE',  ( 1.000000000000000000, 0.000000000000000000, 0.000000000000000000 ) ) ;
#2299 = CARTESIAN_POINT ( 'NONE',  ( 0.02436607992776238310, -12.59161484032927092, 21.30679549418627161 ) ) ;
#2300 = EDGE_LOOP ( 'NONE', ( #12748, #556, #6236, #6495 ) ) ;
#2301 = EDGE_CURVE ( 'NONE', #6946, #2063, #10610, .T. ) ;
#2302 = SURFACE_SIDE_STYLE ('',( #12976 ) ) ;
#2303 = ORIENTED_EDGE ( 'NONE', *, *, #4453, .F. ) ;
#2304 = ORIENTED_EDGE ( 'NONE', *, *, #1712, .T. ) ;
#2305 = ORIENTED_EDGE ( 'NONE', *, *, #376, .T. ) ;
#2306 = CARTESIAN_POINT ( 'NONE',  ( 0.02436607992776281678, 2.336989772644269436, 24.63872515616083447 ) ) ;
#2307 =( NAMED_UNIT ( * ) SI_UNIT ( $, .STERADIAN. ) SOLID_ANGLE_UNIT ( ) );
#2308 = EDGE_CURVE ( 'NONE', #15036, #14991, #9612, .T. ) ;
#2309 = CARTESIAN_POINT ( 'NONE',  ( 0.02531912748464674665, 5.229914364928542447, -13.68080036884343009 ) ) ;
#2310 = CYLINDRICAL_SURFACE ( 'NONE', #12232, 7.000000000000000000 ) ;
#2311 = AXIS2_PLACEMENT_3D ( 'NONE', #5729, #1186, #3418 ) ;
#2313 = AXIS2_PLACEMENT_3D ( 'NONE', #4662, #2489, #5948 ) ;
#2312 = CARTESIAN_POINT ( 'NONE',  ( 0.5431871198829543168, -3.619024283481952597, -16.57708379306448165 ) ) ;
#2314 = ORIENTED_EDGE ( 'NONE', *, *, #3325, .F. ) ;
#2315 = DIRECTION ( 'NONE',  ( 1.000000000000000000, -0.000000000000000000, -0.000000000000000000 ) ) ;
#2316 = PRODUCT_RELATED_PRODUCT_CATEGORY ( 'part', '', ( #9463 ) ) ;
#2317 = ADVANCED_FACE ( 'NONE', ( #7046 ), #3504, .T. ) ;
#2318 = EDGE_CURVE ( 'NONE', #13976, #8350, #7453, .T. ) ;
#2319 = VECTOR ( 'NONE', #61, 1000.000000000000000 ) ;
#2320 = CIRCLE ( 'NONE', #10417, 20.00000000000000000 ) ;
#2321 =( REPRESENTATION_RELATIONSHIP ('NONE','NONE', #12685, #7891 ) REPRESENTATION_RELATIONSHIP_WITH_TRANSFORMATION ( #4443 )SHAPE_REPRESENTATION_RELATIONSHIP( ) );
#2322 = ORIENTED_EDGE ( 'NONE', *, *, #1019, .F. ) ;
#2323 = CARTESIAN_POINT ( 'NONE',  ( 1.749999999999999778, 0.000000000000000000, 0.000000000000000000 ) ) ;
#2324 = CARTESIAN_POINT ( 'NONE',  ( 2.790000000000077751, -24.22524813288760370, -2.133839912091053836 ) ) ;
#2325 = ORIENTED_EDGE ( 'NONE', *, *, #10306, .F. ) ;
#2326 = ORIENTED_EDGE ( 'NONE', *, *, #12496, .F. ) ;
#2327 = DIRECTION ( 'NONE',  ( 0.000000000000000000, 0.000000000000000000, 1.000000000000000000 ) ) ;
#2328 = AXIS2_PLACEMENT_3D ( 'NONE', #7519, #12342, #12193 ) ;
#2329 = EDGE_CURVE ( 'NONE', #1136, #13200, #12726, .T. ) ;
#2330 = ORIENTED_EDGE ( 'NONE', *, *, #10701, .F. ) ;
#2331 = AXIS2_PLACEMENT_3D ( 'NONE', #8, #10391, #11614 ) ;
#2332 = DIRECTION ( 'NONE',  ( -0.000000000000000000, -1.000000000000000000, -0.000000000000000000 ) ) ;
#2333 = FACE_OUTER_BOUND ( 'NONE', #13646, .T. ) ;
#2334 = B_SPLINE_CURVE_WITH_KNOTS ( 'NONE', 3,
 ( #8832, #451, #5092, #13526 ),
 .UNSPECIFIED., .F., .F.,
 ( 4, 4 ),
 ( 2.451234579287542699E-07, 0.0006917187676826530357 ),
 .UNSPECIFIED. ) ;
#2335 = ADVANCED_FACE ( 'NONE', ( #5901 ), #9415, .F. ) ;
#2336 = CYLINDRICAL_SURFACE ( 'NONE', #11386, 4.000000000000000000 ) ;
#2337 = CARTESIAN_POINT ( 'NONE',  ( 2.789999999999999147, -5.456805104201270851, 23.69843731927166885 ) ) ;
#2338 = ORIENTED_EDGE ( 'NONE', *, *, #3364, .T. ) ;
#2339 = DIRECTION ( 'NONE',  ( -0.000000000000000000, -0.000000000000000000, -1.000000000000000000 ) ) ;
#2340 = DIRECTION ( 'NONE',  ( 1.000000000000000000, 0.000000000000000000, 0.000000000000000000 ) ) ;
#2341 = ORIENTED_EDGE ( 'NONE', *, *, #7033, .F. ) ;
#2342 = AXIS2_PLACEMENT_3D ( 'NONE', #1319, #8384, #9549 ) ;
#2343 = ADVANCED_FACE ( 'NONE', ( #11864 ), #11794, .T. ) ;
#2344 = AXIS2_PLACEMENT_3D ( 'NONE', #1397, #7090, #2479 ) ;
#2345 = ORIENTED_EDGE ( 'NONE', *, *, #10163, .F. ) ;
#2346 = CARTESIAN_POINT ( 'NONE',  ( 0.7686372590627849055, -5.021526291670431519, 16.74220655292935334 ) ) ;
#2347 = DIRECTION ( 'NONE',  ( -1.000000000000000000, 0.000000000000000000, -0.000000000000000000 ) ) ;
#2348 = CARTESIAN_POINT ( 'NONE',  ( 2.246812850058911071, 5.154374911958910843, 16.16568790143443479 ) ) ;
#2349 = CARTESIAN_POINT ( 'NONE',  ( 2.789999999999999147, -16.37294372382844543, -18.55949924794910544 ) ) ;
#2350 = ITEM_DEFINED_TRANSFORMATION ( 'NONE', 'NONE', #4762,  #1376 ) ;
#2351 = PLANE ( 'NONE',  #11505 ) ;
#2352 = CARTESIAN_POINT ( 'NONE',  ( 0.000000000000000000, -12.52067188844335988, -20.62201879784928238 ) ) ;
#2353 = VECTOR ( 'NONE', #6220, 1000.000000000000000 ) ;
#2354 = ORIENTED_EDGE ( 'NONE', *, *, #6108, .T. ) ;
#2355 = FACE_OUTER_BOUND ( 'NONE', #12520, .T. ) ;
#2356 = CARTESIAN_POINT ( 'NONE',  ( 20.40394475573011590, -10.79473832354794460, 22.47056274847713908 ) ) ;
#2357 = DIRECTION ( 'NONE',  ( 0.4571871344001383619, 0.8893705212896307888, 0.000000000000000000 ) ) ;
#2358 = CARTESIAN_POINT ( 'NONE',  ( 0.000000000000000000, 15.74360496233409634, -18.28042085475261302 ) ) ;
#2359 = VERTEX_POINT ( 'NONE', #8267 ) ;
#2360 = VERTEX_POINT ( 'NONE', #12949 ) ;
#2361 = TOROIDAL_SURFACE ( 'NONE', #647, 14.01039946648074341, 8.000000000000000000 ) ;
#2362 = CYLINDRICAL_SURFACE ( 'NONE', #1092, 13.19999999999999929 ) ;
#2363 = ORIENTED_EDGE ( 'NONE', *, *, #4205, .F. ) ;
#2364 = CARTESIAN_POINT ( 'NONE',  ( 2.010451923687323728, 12.70439593876677620, -11.98750039041481408 ) ) ;
#2365 = AXIS2_PLACEMENT_3D ( 'NONE', #14254, #13975, #4962 ) ;
#2366 = FACE_OUTER_BOUND ( 'NONE', #7966, .T. ) ;
#2367 = MECHANICAL_DESIGN_GEOMETRIC_PRESENTATION_REPRESENTATION (  '', ( #1143 ), #8251 ) ;
#2368 = LINE ( 'NONE', #7203, #7795 ) ;
#2369 = DIRECTION ( 'NONE',  ( 0.000000000000000000, 0.000000000000000000, 1.000000000000000000 ) ) ;
#2370 = CARTESIAN_POINT ( 'NONE',  ( 2.718184743034449014, 5.344212458769360907, 24.78695292654923676 ) ) ;
#2371 = CARTESIAN_POINT ( 'NONE',  ( 2.764680872513682885, -14.46287784598619020, 2.311161484776505404 ) ) ;
#2372 = DIRECTION ( 'NONE',  ( 1.000000000000000000, 0.000000000000000000, 0.000000000000000000 ) ) ;
#2373 = EDGE_LOOP ( 'NONE', ( #4963, #5156, #10411, #2444, #7197, #1961, #1248, #9854 ) ) ;
#2374 = AXIS2_PLACEMENT_3D ( 'NONE', #1351, #3662, #3731 ) ;
#2375 = TOROIDAL_SURFACE ( 'NONE', #1151, 24.12539914357697413, 8.000000000000000000 ) ;
#2376 = CARTESIAN_POINT ( 'NONE',  ( 0.000000000000000000, 0.000000000000000000, 1.395000000000000462 ) ) ;
#2377 =( NAMED_UNIT ( * ) SI_UNIT ( $, .STERADIAN. ) SOLID_ANGLE_UNIT ( ) );
#2378 = EDGE_CURVE ( 'NONE', #13028, #6156, #2757, .T. ) ;
#2379 = ORIENTED_EDGE ( 'NONE', *, *, #11552, .T. ) ;
#2380 = AXIS2_PLACEMENT_3D ( 'NONE', #12215, #1694, #6377 ) ;
#2381 = VECTOR ( 'NONE', #10886, 1000.000000000000000 ) ;
#2382 =( NAMED_UNIT ( * ) SI_UNIT ( $, .STERADIAN. ) SOLID_ANGLE_UNIT ( ) );
#2383 = VERTEX_POINT ( 'NONE', #14268 ) ;
#2384 = ORIENTED_EDGE ( 'NONE', *, *, #8908, .T. ) ;
#2385 = ORIENTED_EDGE ( 'NONE', *, *, #2155, .T. ) ;
#2386 = CYLINDRICAL_SURFACE ( 'NONE', #905, 8.400000000000000355 ) ;
#2387 = CARTESIAN_POINT ( 'NONE',  ( 0.02531912748679390063, 9.232963481057920418, -11.36963888406677725 ) ) ;
#2388 = AXIS2_PLACEMENT_3D ( 'NONE', #6723, #11403, #738 ) ;
#2389 = B_SPLINE_CURVE_WITH_KNOTS ( 'NONE', 3,
 ( #7204, #12035, #2594, #11959 ),
 .UNSPECIFIED., .F., .F.,
 ( 4, 4 ),
 ( 2.324263106244727961E-07, 0.0006888201370294890283 ),
 .UNSPECIFIED. ) ;
#2390 = FACE_OUTER_BOUND ( 'NONE', #5694, .T. ) ;
#2391 = DIRECTION ( 'NONE',  ( -1.000000000000000000, 0.000000000000000000, 0.000000000000000000 ) ) ;
#2392 = EDGE_CURVE ( 'NONE', #7949, #448, #8877, .T. ) ;
#2393 = AXIS2_PLACEMENT_3D ( 'NONE', #1217, #10439, #7132 ) ;
#2394 = CARTESIAN_POINT ( 'NONE',  ( 2.789999999999999147, -18.55949924794880346, -16.37294372382878649 ) ) ;
#2395 = CIRCLE ( 'NONE', #2159, 2.524999999999995914 ) ;
#2396 = EDGE_CURVE ( 'NONE', #8331, #14360, #13297, .T. ) ;
#2397 = ORIENTED_EDGE ( 'NONE', *, *, #13935, .F. ) ;
#2398 = VECTOR ( 'NONE', #13030, 1000.000000000000000 ) ;
#2399 = CARTESIAN_POINT ( 'NONE',  ( 2.789999999999999147, 0.000000000000000000, 0.000000000000000000 ) ) ;
#2400 = AXIS2_PLACEMENT_3D ( 'NONE', #11777, #3556, #953 ) ;
#2401 = EDGE_CURVE ( 'NONE', #14060, #1181, #1131, .T. ) ;
#2402 = CIRCLE ( 'NONE', #14437, 6.000000000000005329 ) ;
#2403 = ORIENTED_EDGE ( 'NONE', *, *, #11173, .F. ) ;
#2404 = DIRECTION ( 'NONE',  ( 0.000000000000000000, 1.000000000000000000, -1.224646799147353207E-16 ) ) ;
#2405 = CARTESIAN_POINT ( 'NONE',  ( 0.000000000000000000, 3.361026734705063745E-15, 7.799999999999990052 ) ) ;
#2406 = AXIS2_PLACEMENT_3D ( 'NONE', #11566, #11272, #2045 ) ;
#2407 = EDGE_LOOP ( 'NONE', ( #8366, #13231, #9644, #13437 ) ) ;
#2408 = ORIENTED_EDGE ( 'NONE', *, *, #10953, .F. ) ;
#2409 = EDGE_CURVE ( 'NONE', #5354, #6094, #8376, .T. ) ;
#2410 = DIRECTION ( 'NONE',  ( 1.000000000000000000, 0.000000000000000000, 0.000000000000000000 ) ) ;
#2411 = ORIENTED_EDGE ( 'NONE', *, *, #8973, .T. ) ;
#2412 = CARTESIAN_POINT ( 'NONE',  ( 2.764680872513682441, -2.311161484776455222, -14.46287784598619908 ) ) ;
#2413 = AXIS2_PLACEMENT_3D ( 'NONE', #8905, #2769, #2926 ) ;
#2414 = CARTESIAN_POINT ( 'NONE',  ( -4.000000000000000888, 0.000000000000000000, 10.00000000000000000 ) ) ;
#2415 = DIRECTION ( 'NONE',  ( -1.000000000000000000, -0.000000000000000000, -0.000000000000000000 ) ) ;
#2416 = CARTESIAN_POINT ( 'NONE',  ( 74.00000000000000000, 0.000000000000000000, 3.000000000000000000 ) ) ;
#2417 = EDGE_CURVE ( 'NONE', #6870, #10268, #1347, .T. ) ;
#2418 = AXIS2_PLACEMENT_3D ( 'NONE', #5707, #13632, #1801 ) ;
#2419 = ORIENTED_EDGE ( 'NONE', *, *, #8213, .T. ) ;
#2420 = VECTOR ( 'NONE', #10730, 1000.000000000000000 ) ;
#2421 = CARTESIAN_POINT ( 'NONE',  ( -10.40394475573011945, -10.79473832354794460, -3.532509375119139690E-15 ) ) ;
#2422 = CARTESIAN_POINT ( 'NONE',  ( 84.00000000000000000, 0.000000000000000000, 5.500000000000005329 ) ) ;
#2423 = ORIENTED_EDGE ( 'NONE', *, *, #8775, .T. ) ;
#2424 = EDGE_CURVE ( 'NONE', #7858, #10809, #8639, .T. ) ;
#2425 = ORIENTED_EDGE ( 'NONE', *, *, #14370, .F. ) ;
#2426 = CARTESIAN_POINT ( 'NONE',  ( 0.09203968221122213467, -5.280991956247218511, 14.31435947614540538 ) ) ;
#2427 = DIRECTION ( 'NONE',  ( -1.000000000000000000, 0.000000000000000000, -0.000000000000000000 ) ) ;
#2428 = ADVANCED_FACE ( 'NONE', ( #9579 ), #8053, .T. ) ;
#2429 = EDGE_CURVE ( 'NONE', #7404, #12603, #10351, .T. ) ;
#2430 = CARTESIAN_POINT ( 'NONE',  ( 0.000000000000000000, 7.909232158575156824, -24.34211360614291664 ) ) ;
#2431 = CARTESIAN_POINT ( 'NONE',  ( 8.000000000000000000, 0.000000000000000000, 0.000000000000000000 ) ) ;
#2432 = VECTOR ( 'NONE', #3661, 1000.000000000000000 ) ;
#2434 = CARTESIAN_POINT ( 'NONE',  ( 2.262072706628476926, -18.56460150496924655, -19.66369668717053898 ) ) ;
#2433 = AXIS2_PLACEMENT_3D ( 'NONE', #2124, #4741, #7117 ) ;
#2435 = CARTESIAN_POINT ( 'NONE',  ( 2.597943646031689813, 2.883512197589014558, 15.58455734132167869 ) ) ;
#2436 = ORIENTED_EDGE ( 'NONE', *, *, #14820, .F. ) ;
#2437 = FACE_BOUND ( 'NONE', #12966, .T. ) ;
#2438 = DIRECTION ( 'NONE',  ( -1.000000000000000000, 0.000000000000000000, 0.000000000000000000 ) ) ;
#2439 = DIRECTION ( 'NONE',  ( 0.000000000000000000, 0.000000000000000000, 1.000000000000000000 ) ) ;
#2440 = DIRECTION ( 'NONE',  ( 0.000000000000000000, 0.000000000000000000, 1.000000000000000000 ) ) ;
#2441 = VERTEX_POINT ( 'NONE', #12795 ) ;
#2442 = EDGE_CURVE ( 'NONE', #11373, #2185, #2283, .T. ) ;
#2443 = CIRCLE ( 'NONE', #11027, 5.999999999999999112 ) ;
#2444 = ORIENTED_EDGE ( 'NONE', *, *, #6440, .T. ) ;
#2445 = EDGE_CURVE ( 'NONE', #960, #1432, #3722, .T. ) ;
#2446 = CARTESIAN_POINT ( 'NONE',  ( 1.039999999999995817, 27.76164181293051669, 4.147968289691385202 ) ) ;
#2447 = ORIENTED_EDGE ( 'NONE', *, *, #6573, .T. ) ;
#2448 = CARTESIAN_POINT ( 'NONE',  ( 0.04999670013151677472, 9.490919315500136122, 11.55877992729668691 ) ) ;
#2449 = DIRECTION ( 'NONE',  ( 1.000000000000000000, 0.000000000000000000, 0.000000000000000000 ) ) ;
#2450 = ADVANCED_FACE ( 'NONE', ( #493 ), #14507, .F. ) ;
#2451 = DIRECTION ( 'NONE',  ( -1.000000000000000000, -0.000000000000000000, 0.000000000000000000 ) ) ;
#2452 = DIRECTION ( 'NONE',  ( -1.000000000000000000, -0.000000000000000000, -0.000000000000000000 ) ) ;
#2453 = CARTESIAN_POINT ( 'NONE',  ( 80.00000000000000000, 0.000000000000000000, -1.395000000000000462 ) ) ;
#2454 = DIRECTION ( 'NONE',  ( 0.000000000000000000, 0.000000000000000000, -1.000000000000000000 ) ) ;
#2455 = VERTEX_POINT ( 'NONE', #13412 ) ;
#2456 = DIRECTION ( 'NONE',  ( -0.000000000000000000, 1.000000000000000000, -0.000000000000000000 ) ) ;
#2457 = CARTESIAN_POINT ( 'NONE',  ( -20.63749999999999574, 6.827405905246494173E-16, 5.575000000000000178 ) ) ;
#2458 = VECTOR ( 'NONE', #3595, 1000.000000000000000 ) ;
#2459 = ADVANCED_FACE ( 'NONE', ( #5056 ), #13182, .F. ) ;
#2460 = ORIENTED_EDGE ( 'NONE', *, *, #11205, .F. ) ;
#2461 = CARTESIAN_POINT ( 'NONE',  ( 0.000000000000000000, 0.000000000000000000, 0.000000000000000000 ) ) ;
#2462 = LINE ( 'NONE', #11816, #4829 ) ;
#2463 = CARTESIAN_POINT ( 'NONE',  ( 6.000000000000000888, 0.000000000000000000, 7.000000000000000000 ) ) ;
#2464 = ORIENTED_EDGE ( 'NONE', *, *, #795, .F. ) ;
#2465 = SURFACE_SIDE_STYLE ('',( #10677 ) ) ;
#2466 = ORIENTED_EDGE ( 'NONE', *, *, #8770, .F. ) ;
#2467 = ORIENTED_EDGE ( 'NONE', *, *, #12952, .F. ) ;
#2468 = ORIENTED_EDGE ( 'NONE', *, *, #14073, .T. ) ;
#2469 = DIRECTION ( 'NONE',  ( -0.1643989873053570416, 0.9863939238321438596, 0.000000000000000000 ) ) ;
#2470 = DIRECTION ( 'NONE',  ( -1.000000000000000000, 0.000000000000000000, 0.000000000000000000 ) ) ;
#2471 = CARTESIAN_POINT ( 'NONE',  ( 13.28797974610715116, -21.11867004231547540, 4.000000000000000000 ) ) ;
#2472 = CARTESIAN_POINT ( 'NONE',  ( 2.697960337741385217, -2.583706482362138512, 15.03709480088670603 ) ) ;
#2473 = CARTESIAN_POINT ( 'NONE',  ( 0.7795480803411065640, -4.029281904976750539, 16.99607982911240001 ) ) ;
#2474 = B_SPLINE_CURVE_WITH_KNOTS ( 'NONE', 3,
 ( #11763, #4784, #4713, #9321, #141, #9454 ),
 .UNSPECIFIED., .F., .F.,
 ( 4, 2, 4 ),
 ( 1.979325885386966398E-07, 0.001878588715165604951, 0.003756979497742671432 ),
 .UNSPECIFIED. ) ;
#2475 = VERTEX_POINT ( 'NONE', #9728 ) ;
#2476 = DIRECTION ( 'NONE',  ( -1.000000000000000000, 0.000000000000000000, 0.000000000000000000 ) ) ;
#2477 = B_SPLINE_CURVE_WITH_KNOTS ( 'NONE', 3,
 ( #7391, #2924, #3995, #9764 ),
 .UNSPECIFIED., .F., .F.,
 ( 4, 4 ),
 ( 0.005258105385878691744, 0.005948373736081389272 ),
 .UNSPECIFIED. ) ;
#2478 = ORIENTED_EDGE ( 'NONE', *, *, #10100, .F. ) ;
#2479 = DIRECTION ( 'NONE',  ( 0.000000000000000000, 0.000000000000000000, 1.000000000000000000 ) ) ;
#2480 = PRODUCT ( 'plate 1', 'plate 1', '', ( #7597 ) ) ;
#2481 = EDGE_CURVE ( 'NONE', #7818, #1860, #5212, .T. ) ;
#2482 = DIRECTION ( 'NONE',  ( -1.000000000000000000, -0.000000000000000000, -0.000000000000000000 ) ) ;
#2483 = ORIENTED_EDGE ( 'NONE', *, *, #12170, .T. ) ;
#2484 = ORIENTED_EDGE ( 'NONE', *, *, #932, .T. ) ;
#2485 = CARTESIAN_POINT ( 'NONE',  ( 88.46153288930041469, 16.46030115554384565, 2.999999999999999112 ) ) ;
#2486 = ORIENTED_EDGE ( 'NONE', *, *, #180, .T. ) ;
#2487 = CYLINDRICAL_SURFACE ( 'NONE', #9206, 2.524999999999995914 ) ;
#2488 = CARTESIAN_POINT ( 'NONE',  ( 0.02436607992776021470, 21.30679549418649543, -12.59161484032888723 ) ) ;
#2489 = DIRECTION ( 'NONE',  ( 0.000000000000000000, 0.000000000000000000, 1.000000000000000000 ) ) ;
#2490 = VERTEX_POINT ( 'NONE', #3806 ) ;
#2491 = CARTESIAN_POINT ( 'NONE',  ( -16.23224367729419271, -7.237025146040848789, -5.000000000000000000 ) ) ;
#2492 = DIRECTION ( 'NONE',  ( 1.000000000000000000, -0.000000000000000000, -0.000000000000000000 ) ) ;
#2493 = ORIENTED_EDGE ( 'NONE', *, *, #4742, .F. ) ;
#2494 = VERTEX_POINT ( 'NONE', #9875 ) ;
#2495 = ORIENTED_EDGE ( 'NONE', *, *, #5362, .T. ) ;
#2496 = CARTESIAN_POINT ( 'NONE',  ( 0.9041604711286037599, -12.77651625388890544, -12.27244837507626585 ) ) ;
#2497 = CARTESIAN_POINT ( 'NONE',  ( 0.000000000000000000, -5.535312321042547445, -23.48180575137738302 ) ) ;
#2498 = VECTOR ( 'NONE', #6820, 1000.000000000000000 ) ;
#2499 = ADVANCED_FACE ( 'NONE', ( #2740 ), #13092, .F. ) ;
#2500 = CARTESIAN_POINT ( 'NONE',  ( 1.749999999999998002, 0.000000000000000000, 0.000000000000000000 ) ) ;
#2501 = CARTESIAN_POINT ( 'NONE',  ( 98.48580539929344013, 0.9022481406819604643, 2.999999999999999112 ) ) ;
#2502 = CONTEXT_DEPENDENT_SHAPE_REPRESENTATION ( #8809, #7994 ) ;
#2503 = DIRECTION ( 'NONE',  ( -0.9863939238321437486, -0.1643989873053572359, 0.000000000000000000 ) ) ;
#2504 = CARTESIAN_POINT ( 'NONE',  ( 2.789999999999999147, 0.000000000000000000, 0.000000000000000000 ) ) ;
#2505 = ORIENTED_EDGE ( 'NONE', *, *, #14754, .T. ) ;
#2506 = DIRECTION ( 'NONE',  ( 0.000000000000000000, 0.000000000000000000, 1.000000000000000000 ) ) ;
#2507 = CARTESIAN_POINT ( 'NONE',  ( 2.789999999999999147, -24.44424927289185590, -0.2301004812060095106 ) ) ;
#2508 = DIRECTION ( 'NONE',  ( 0.000000000000000000, -0.8090169943749488946, 0.5877852522924711387 ) ) ;
#2509 = FACE_OUTER_BOUND ( 'NONE', #1196, .T. ) ;
#2510 = EDGE_CURVE ( 'NONE', #1861, #4961, #11576, .T. ) ;
#2511 = AXIS2_PLACEMENT_3D ( 'NONE', #8718, #9956, #1434 ) ;
#2512 = EDGE_CURVE ( 'NONE', #12014, #2008, #6927, .T. ) ;
#2513 = ORIENTED_EDGE ( 'NONE', *, *, #10110, .F. ) ;
#2514 = ORIENTED_EDGE ( 'NONE', *, *, #9096, .T. ) ;
#2515 = VERTEX_POINT ( 'NONE', #9810 ) ;
#2516 = CARTESIAN_POINT ( 'NONE',  ( 2.337784053193427969, 12.42068120944096776, -11.13074453164190913 ) ) ;
#2517 = FACE_OUTER_BOUND ( 'NONE', #8195, .T. ) ;
#2518 = CARTESIAN_POINT ( 'NONE',  ( 2.789999999999999147, 9.232963481057920418, -11.36963888406677725 ) ) ;
#2519 = CARTESIAN_POINT ( 'NONE',  ( 0.5279273746168618997, -26.57710921259763737, 4.996265754456265640 ) ) ;
#2520 = DIRECTION ( 'NONE',  ( 1.000000000000000000, 0.000000000000000000, 0.000000000000000000 ) ) ;
#2521 = DIRECTION ( 'NONE',  ( -0.9863939238321437486, -0.1643989873053572359, 0.000000000000000000 ) ) ;
#2522 = AXIS2_PLACEMENT_3D ( 'NONE', #3024, #11541, #8010 ) ;
#2523 = ORIENTED_EDGE ( 'NONE', *, *, #1156, .F. ) ;
#2524 = CARTESIAN_POINT ( 'NONE',  ( 2.789999999999999147, 7.909232158574813099, 24.34211360614303388 ) ) ;
#2525 = DIRECTION ( 'NONE',  ( -1.000000000000000000, -0.000000000000000000, -0.000000000000000000 ) ) ;
#2526 = EDGE_CURVE ( 'NONE', #2359, #3152, #13260, .T. ) ;
#2527 = EDGE_CURVE ( 'NONE', #13334, #8127, #4234, .T. ) ;
#2528 = ORIENTED_EDGE ( 'NONE', *, *, #5262, .F. ) ;
#2529 = CARTESIAN_POINT ( 'NONE',  ( 0.07181524296601557444, 18.89296398180216130, -16.91181672897712929 ) ) ;
#2530 = LINE ( 'NONE', #13990, #14147 ) ;
#2531 = EDGE_CURVE ( 'NONE', #10080, #212, #12324, .T. ) ;
#2532 = ORIENTED_EDGE ( 'NONE', *, *, #9310, .F. ) ;
#2533 = ORIENTED_EDGE ( 'NONE', *, *, #14679, .F. ) ;
#2534 = VERTEX_POINT ( 'NONE', #11102 ) ;
#2535 = ORIENTED_EDGE ( 'NONE', *, *, #5195, .T. ) ;
#2536 = FACE_OUTER_BOUND ( 'NONE', #4180, .T. ) ;
#2537 = CARTESIAN_POINT ( 'NONE',  ( 2.601776091974069782, -25.40949241676357317, 5.251266773802275800 ) ) ;
#2538 = EDGE_CURVE ( 'NONE', #1940, #7326, #14049, .T. ) ;
#2539 = DIRECTION ( 'NONE',  ( 1.000000000000000000, 0.000000000000000000, 0.000000000000000000 ) ) ;
#2540 = CARTESIAN_POINT ( 'NONE',  ( 2.010451923687323283, -11.98750039041484783, -12.70439593876673001 ) ) ;
#2541 = CARTESIAN_POINT ( 'NONE',  ( 0.000000000000000000, 0.000000000000000000, 0.000000000000000000 ) ) ;
#2542 = ORIENTED_EDGE ( 'NONE', *, *, #11030, .T. ) ;
#2543 = DIRECTION ( 'NONE',  ( 0.6743761619433820131, 0.7383879686198261405, -5.947623346206184252E-19 ) ) ;
#2544 = AXIS2_PLACEMENT_3D ( 'NONE', #1596, #3744, #201 ) ;
#2545 = ORIENTED_EDGE ( 'NONE', *, *, #14478, .F. ) ;
#2546 = DIRECTION ( 'NONE',  ( 5.782411586589355667E-16, 1.000000000000000000, 0.000000000000000000 ) ) ;
#2547 = PLANE ( 'NONE',  #6503 ) ;
#2548 = VERTEX_POINT ( 'NONE', #564 ) ;
#2549 = VECTOR ( 'NONE', #13472, 999.9999999999998863 ) ;
#2550 = ORIENTED_EDGE ( 'NONE', *, *, #1457, .T. ) ;
#2551 = CIRCLE ( 'NONE', #4040, 3.000000000000002665 ) ;
#2552 = CARTESIAN_POINT ( 'NONE',  ( 2.789999999999999147, -9.324097380959294412, -22.25075486061747654 ) ) ;
#2553 = VERTEX_POINT ( 'NONE', #7583 ) ;
#2554 = DIRECTION ( 'NONE',  ( 0.000000000000000000, 0.000000000000000000, 1.000000000000000000 ) ) ;
#2555 = DIRECTION ( 'NONE',  ( -1.000000000000000000, 0.000000000000000000, 0.000000000000000000 ) ) ;
#2556 = CIRCLE ( 'NONE', #9685, 4.872650870659752442 ) ;
#2557 = CARTESIAN_POINT ( 'NONE',  ( 18.21994936526786901, -20.29667510578869027, 4.000000000000000000 ) ) ;
#2558 = LINE ( 'NONE', #6539, #4527 ) ;
#2559 = AXIS2_PLACEMENT_3D ( 'NONE', #8822, #6441, #9832 ) ;
#2560 = ORIENTED_EDGE ( 'NONE', *, *, #11056, .F. ) ;
#2561 = DIRECTION ( 'NONE',  ( 0.000000000000000000, 0.000000000000000000, 1.000000000000000000 ) ) ;
#2562 = ADVANCED_FACE ( 'NONE', ( #13330 ), #6268, .F. ) ;
#2563 = LINE ( 'NONE', #11928, #3125 ) ;
#2564 = ORIENTED_EDGE ( 'NONE', *, *, #14781, .F. ) ;
#2565 = DIRECTION ( 'NONE',  ( 0.000000000000000000, -0.5877852522924684742, -0.8090169943749507819 ) ) ;
#2566 = ORIENTED_EDGE ( 'NONE', *, *, #4687, .F. ) ;
#2567 = VERTEX_POINT ( 'NONE', #6123 ) ;
#2568 = CYLINDRICAL_SURFACE ( 'NONE', #9771, 6.000000000000005329 ) ;
#2569 = CARTESIAN_POINT ( 'NONE',  ( 0.02436607992775891365, -24.63872515616080960, -2.336989772644527008 ) ) ;
#2570 = AXIS2_PLACEMENT_3D ( 'NONE', #3704, #11841, #2554 ) ;
#2571 = CIRCLE ( 'NONE', #3066, 4.000000000000000000 ) ;
#2572 = CARTESIAN_POINT ( 'NONE',  ( 2.582362639458681386, 5.278564329441002734, 14.94126095370962837 ) ) ;
#2573 = CARTESIAN_POINT ( 'NONE',  ( 13.45237873341251067, -22.10506396614762537, 4.000000000000000000 ) ) ;
#2574 = CARTESIAN_POINT ( 'NONE',  ( 2.789999999999999147, -13.40591150984231916, 7.739906618939660810 ) ) ;
#2575 = EDGE_CURVE ( 'NONE', #4314, #154, #2808, .T. ) ;
#2576 = CARTESIAN_POINT ( 'NONE',  ( 0.000000000000000000, -24.04302995059965653, -1.991882183130557094 ) ) ;
#2577 = EDGE_CURVE ( 'NONE', #11593, #4343, #3734, .T. ) ;
#2578 = ORIENTED_EDGE ( 'NONE', *, *, #3073, .T. ) ;
#2579 = CARTESIAN_POINT ( 'NONE',  ( 1.150000000000001688, 0.000000000000000000, 0.000000000000000000 ) ) ;
#2580 = DIRECTION ( 'NONE',  ( -0.9873505073845697533, 0.1585527532634883052, 0.000000000000000000 ) ) ;
#2581 = CARTESIAN_POINT ( 'NONE',  ( 2.715264205769515105, -2.569134216958794070, -15.04916547791957271 ) ) ;
#2582 = CIRCLE ( 'NONE', #6514, 3.799999999999999378 ) ;
#2583 = FACE_OUTER_BOUND ( 'NONE', #2300, .T. ) ;
#2584 = VECTOR ( 'NONE', #1245, 1000.000000000000000 ) ;
#2585 = ORIENTED_EDGE ( 'NONE', *, *, #5962, .T. ) ;
#2586 = AXIS2_PLACEMENT_3D ( 'NONE', #948, #4567, #6788 ) ;
#2587 = EDGE_CURVE ( 'NONE', #6626, #2812, #9144, .T. ) ;
#2588 = SHAPE_REPRESENTATION ( 'plate 2', ( #1376 ), #5367 ) ;
#2589 = EDGE_LOOP ( 'NONE', ( #11388, #9055, #927, #8161 ) ) ;
#2590 = VERTEX_POINT ( 'NONE', #1807 ) ;
#2591 = DIRECTION ( 'NONE',  ( 0.000000000000000000, 0.000000000000000000, 1.000000000000000000 ) ) ;
#2592 = DIRECTION ( 'NONE',  ( -1.000000000000000000, 0.000000000000000000, 0.000000000000000000 ) ) ;
#2593 = CARTESIAN_POINT ( 'NONE',  ( 18.71314632718394222, -23.25585687728512241, -2.000000000000000000 ) ) ;
#2594 = CARTESIAN_POINT ( 'NONE',  ( 2.790000000000079527, -15.96555658743774941, 18.34439787333500860 ) ) ;
#2595 = CARTESIAN_POINT ( 'NONE',  ( 0.000000000000000000, 0.000000000000000000, 5.750000000000001776 ) ) ;
#2596 = CARTESIAN_POINT ( 'NONE',  ( 2.764680872513933796, 5.229914364928542447, -13.68080036884343009 ) ) ;
#2597 = EDGE_CURVE ( 'NONE', #860, #3207, #5585, .T. ) ;
#2598 = EDGE_CURVE ( 'NONE', #14375, #406, #8802, .T. ) ;
#2599 = ORIENTED_EDGE ( 'NONE', *, *, #10498, .F. ) ;
#2600 = CARTESIAN_POINT ( 'NONE',  ( 72.49759028996474797, 17.18292470770558822, 3.000000000000000000 ) ) ;
#2601 = CARTESIAN_POINT ( 'NONE',  ( 0.02436607992776368414, -9.836394144775550075, -22.71065055754462492 ) ) ;
#2602 = EDGE_LOOP ( 'NONE', ( #9382, #1287, #4247, #1078 ) ) ;
#2603 = CARTESIAN_POINT ( 'NONE',  ( 2.789999999999999147, -7.739906618939614624, -13.40591150984234581 ) ) ;
#2604 = CARTESIAN_POINT ( 'NONE',  ( 1.749999999999999778, 12.55714665599987079, 12.83329210556836308 ) ) ;
#2605 = PRODUCT_DEFINITION_SHAPE ( 'NONE', 'NONE',  #15233 ) ;
#2606 = AXIS2_PLACEMENT_3D ( 'NONE', #12672, #14922, #7993 ) ;
#2607 = ORIENTED_EDGE ( 'NONE', *, *, #13060, .F. ) ;
#2608 = AXIS2_PLACEMENT_3D ( 'NONE', #2988, #7751, #8897 ) ;
#2609 = DIRECTION ( 'NONE',  ( 0.000000000000000000, 0.000000000000000000, 1.000000000000000000 ) ) ;
#2610 = VERTEX_POINT ( 'NONE', #11484 ) ;
#2611 = MECHANICAL_DESIGN_GEOMETRIC_PRESENTATION_REPRESENTATION (  '', ( #9242 ), #10950 ) ;
#2612 = ORIENTED_EDGE ( 'NONE', *, *, #8379, .F. ) ;
#2613 = ORIENTED_EDGE ( 'NONE', *, *, #6588, .F. ) ;
#2614 = CARTESIAN_POINT ( 'NONE',  ( 2.764680872515352661, -14.46287784598615644, -2.311161484776706576 ) ) ;
#2615 = EDGE_CURVE ( 'NONE', #7149, #4429, #11088, .T. ) ;
#2616 = CARTESIAN_POINT ( 'NONE',  ( 0.000000000000000000, 0.000000000000000000, 4.000000000000000000 ) ) ;
#2617 = CARTESIAN_POINT ( 'NONE',  ( 0.5537796532149699136, 16.55730827443880671, 3.624349476775253986 ) ) ;
#2618 = CYLINDRICAL_SURFACE ( 'NONE', #2073, 17.95481323787947403 ) ;
#2619 = DIRECTION ( 'NONE',  ( 0.000000000000000000, 0.000000000000000000, 1.000000000000000000 ) ) ;
#2620 = ADVANCED_FACE ( 'NONE', ( #14802 ), #7885, .T. ) ;
#2621 = EDGE_CURVE ( 'NONE', #11509, #677, #4484, .T. ) ;
#2622 = AXIS2_PLACEMENT_3D ( 'NONE', #1755, #6439, #11119 ) ;
#2623 = CARTESIAN_POINT ( 'NONE',  ( 2.740003299868484898, 11.55877992729665316, 9.490919315500171649 ) ) ;
#2624 = APPLICATION_CONTEXT ( 'automotive_design' ) ;
#2625 = CIRCLE ( 'NONE', #6053, 1.999999999999998446 ) ;
#2626 = ORIENTED_EDGE ( 'NONE', *, *, #11252, .T. ) ;
#2627 = LINE ( 'NONE', #8453, #11685 ) ;
#2628 = CIRCLE ( 'NONE', #155, 2.524999999999998135 ) ;
#2629 = AXIS2_PLACEMENT_3D ( 'NONE', #634, #5352, #14638 ) ;
#2630 = VERTEX_POINT ( 'NONE', #4272 ) ;
#2631 = ORIENTED_EDGE ( 'NONE', *, *, #5544, .T. ) ;
#2632 = ORIENTED_EDGE ( 'NONE', *, *, #6864, .T. ) ;
#2633 = CARTESIAN_POINT ( 'NONE',  ( 70.16198417812034904, 9.730076655429538590, -2.000000000000000888 ) ) ;
#2634 = CARTESIAN_POINT ( 'NONE',  ( 2.718184767880468478, 23.19431517146933430, 10.24584646439546987 ) ) ;
#2635 = ORIENTED_EDGE ( 'NONE', *, *, #2615, .F. ) ;
#2636 = ORIENTED_EDGE ( 'NONE', *, *, #2950, .F. ) ;
#2637 = VECTOR ( 'NONE', #2746, 1000.000000000000000 ) ;
#2638 = VECTOR ( 'NONE', #13736, 1000.000000000000000 ) ;
#2639 = AXIS2_PLACEMENT_3D ( 'NONE', #6529, #6449, #3072 ) ;
#2640 = CARTESIAN_POINT ( 'NONE',  ( 2.765633920072241736, -9.836394144775550075, -22.71065055754462492 ) ) ;
#2641 = ORIENTED_EDGE ( 'NONE', *, *, #8239, .T. ) ;
#2642 = CARTESIAN_POINT ( 'NONE',  ( 0.000000000000000000, 0.000000000000000000, 0.000000000000000000 ) ) ;
#2643 = CARTESIAN_POINT ( 'NONE',  ( 0.000000000000000000, -13.87420763704360382, -1.948757464274321949 ) ) ;
#2644 = EDGE_CURVE ( 'NONE', #8358, #1528, #8892, .T. ) ;
#2645 = CARTESIAN_POINT ( 'NONE',  ( 2.789999999999999147, 7.739906618939895289, -13.40591150984218416 ) ) ;
#2646 = DIRECTION ( 'NONE',  ( 1.000000000000000000, 0.000000000000000000, 0.000000000000000000 ) ) ;
#2647 = TOROIDAL_SURFACE ( 'NONE', #9756, 14.01039946648074341, 8.000000000000000000 ) ;
#2648 = EDGE_LOOP ( 'NONE', ( #10925, #11074, #517, #8122 ) ) ;
#2649 = VECTOR ( 'NONE', #1199, 1000.000000000000000 ) ;
#2650 = CARTESIAN_POINT ( 'NONE',  ( 1.749999999999998002, 4.147968289691672084, -27.76164181293047406 ) ) ;
#2651 = CARTESIAN_POINT ( 'NONE',  ( 0.000000000000000000, 0.000000000000000000, 3.895000000000000462 ) ) ;
#2652 = CIRCLE ( 'NONE', #14941, 4.000000000000000888 ) ;
#2653 = ORIENTED_EDGE ( 'NONE', *, *, #7297, .T. ) ;
#2654 = CARTESIAN_POINT ( 'NONE',  ( 0.9041604711286033158, 12.77651625388899248, 12.27244837507617881 ) ) ;
#2655 = ORIENTED_EDGE ( 'NONE', *, *, #14537, .T. ) ;
#2656 = VERTEX_POINT ( 'NONE', #2964 ) ;
#2657 = CARTESIAN_POINT ( 'NONE',  ( 2.764680872513208154, 9.232963481057765875, 11.36963888406690870 ) ) ;
#2658 = LINE ( 'NONE', #6929, #4395 ) ;
#2659 = VECTOR ( 'NONE', #12856, 1000.000000000000000 ) ;
#2660 = DIRECTION ( 'NONE',  ( 0.000000000000000000, 0.000000000000000000, 1.000000000000000000 ) ) ;
#2661 = EDGE_CURVE ( 'NONE', #5872, #10328, #6721, .T. ) ;
#2662 = DIRECTION ( 'NONE',  ( -1.000000000000000000, 0.000000000000000000, 0.000000000000000000 ) ) ;
#2663 = AXIS2_PLACEMENT_3D ( 'NONE', #4672, #12787, #11936 ) ;
#2664 = AXIS2_PLACEMENT_3D ( 'NONE', #12025, #5138, #7360 ) ;
#2665 = B_SPLINE_CURVE_WITH_KNOTS ( 'NONE', 3,
 ( #1086, #7158, #2312, #4641, #14304, #7002, #11680, #10690 ),
 .UNSPECIFIED., .F., .F.,
 ( 4, 2, 2, 4 ),
 ( 4.663089412835749521E-07, 0.001898630173449115206, 0.002847712105703030603, 0.003796794037956946217 ),
 .UNSPECIFIED. ) ;
#2666 = ORIENTED_EDGE ( 'NONE', *, *, #1183, .T. ) ;
#2667 = PLANE ( 'NONE',  #12480 ) ;
#2668 = DIRECTION ( 'NONE',  ( -1.000000000000000000, 0.000000000000000000, 0.000000000000000000 ) ) ;
#2669 = FACE_OUTER_BOUND ( 'NONE', #9939, .T. ) ;
#2670 = FACE_OUTER_BOUND ( 'NONE', #10290, .T. ) ;
#2671 = ORIENTED_EDGE ( 'NONE', *, *, #11542, .F. ) ;
#2672 = ORIENTED_EDGE ( 'NONE', *, *, #6777, .F. ) ;
#2673 = EDGE_CURVE ( 'NONE', #5525, #1940, #4244, .T. ) ;
#2674 = ORIENTED_EDGE ( 'NONE', *, *, #1475, .F. ) ;
#2675 = AXIS2_PLACEMENT_3D ( 'NONE', #1580, #13093, #8575 ) ;
#2676 = VECTOR ( 'NONE', #1887, 1000.000000000000000 ) ;
#2677 = DIRECTION ( 'NONE',  ( 0.000000000000000000, 0.000000000000000000, 1.000000000000000000 ) ) ;
#2678 = DIRECTION ( 'NONE',  ( 1.000000000000000000, 0.000000000000000000, 0.000000000000000000 ) ) ;
#2679 = EDGE_CURVE ( 'NONE', #12188, #5632, #12812, .T. ) ;
#2680 = LINE ( 'NONE', #13423, #8264 ) ;
#2681 = CARTESIAN_POINT ( 'NONE',  ( 2.789999999999999147, 12.98979500319694047, 5.249430348645800493 ) ) ;
#2682 = DIRECTION ( 'NONE',  ( 0.000000000000000000, 0.000000000000000000, 1.000000000000000000 ) ) ;
#2683 = CARTESIAN_POINT ( 'NONE',  ( 98.33955663538051795, 3.898681236723621879, 2.999999999999999112 ) ) ;
#2684 = ORIENTED_EDGE ( 'NONE', *, *, #10788, .F. ) ;
#2685 = DIRECTION ( 'NONE',  ( 0.000000000000000000, 0.000000000000000000, -1.000000000000000000 ) ) ;
#2686 = CARTESIAN_POINT ( 'NONE',  ( 2.789999999999999147, -15.04425356660774682, 20.70663861606266209 ) ) ;
#2687 = ORIENTED_EDGE ( 'NONE', *, *, #6331, .F. ) ;
#2688 = CARTESIAN_POINT ( 'NONE',  ( -19.40394475573012301, -16.79473832354794993, 12.00000000000000000 ) ) ;
#2689 = CARTESIAN_POINT ( 'NONE',  ( 2.789999999999999147, 12.52067188844381107, -20.62201879784899461 ) ) ;
#2690 = AXIS2_PLACEMENT_3D ( 'NONE', #3725, #5256, #9926 ) ;
#2691 = CARTESIAN_POINT ( 'NONE',  ( 0.000000000000000000, 1.991882183130641248, -24.04302995059964942 ) ) ;
#2692 = ORIENTED_EDGE ( 'NONE', *, *, #13890, .T. ) ;
#2693 = CARTESIAN_POINT ( 'NONE',  ( 0.2076372544708476597, -12.04200105039477720, 10.30022894898801766 ) ) ;
#2694 = DIRECTION ( 'NONE',  ( 0.000000000000000000, 0.000000000000000000, 1.000000000000000000 ) ) ;
#2695 = ORIENTED_EDGE ( 'NONE', *, *, #14679, .T. ) ;
#2696 = VERTEX_POINT ( 'NONE', #4432 ) ;
#2697 = ORIENTED_EDGE ( 'NONE', *, *, #5601, .T. ) ;
#2698 = SURFACE_STYLE_FILL_AREA ( #2766 ) ;
#2699 = CARTESIAN_POINT ( 'NONE',  ( 2.718131914667133220, 10.24630254990516143, 23.19485392143217339 ) ) ;
#2700 = CARTESIAN_POINT ( 'NONE',  ( 2.246812880117042610, -3.619024283482186632, 16.57708379306443192 ) ) ;
#2701 = AXIS2_PLACEMENT_3D ( 'NONE', #14538, #8610, #9772 ) ;
#2702 = DIRECTION ( 'NONE',  ( 0.000000000000000000, 0.000000000000000000, 1.000000000000000000 ) ) ;
#2703 = ADVANCED_FACE ( 'NONE', ( #653 ), #12631, .T. ) ;
#2704 = CARTESIAN_POINT ( 'NONE',  ( -5.209999999999999964, 0.000000000000000000, 0.000000000000000000 ) ) ;
#2705 = ORIENTED_EDGE ( 'NONE', *, *, #13390, .T. ) ;
#2706 = DIRECTION ( 'NONE',  ( 1.000000000000000000, 0.000000000000000000, 0.000000000000000000 ) ) ;
#2707 = ADVANCED_FACE ( 'NONE', ( #14733 ), #15038, .T. ) ;
#2708 = EDGE_CURVE ( 'NONE', #5145, #10081, #5437, .T. ) ;
#2709 = EDGE_LOOP ( 'NONE', ( #3455, #2098 ) ) ;
#2710 = ORIENTED_EDGE ( 'NONE', *, *, #12921, .F. ) ;
#2711 = CARTESIAN_POINT ( 'NONE',  ( 2.262072637928883800, -23.73240184472485836, -12.96450951081243375 ) ) ;
#2712 = DIRECTION ( 'NONE',  ( -1.000000000000000000, 0.000000000000000000, 0.000000000000000000 ) ) ;
#2713 = EDGE_LOOP ( 'NONE', ( #8843, #12332, #6690, #8767, #1297 ) ) ;
#2714 =( REPRESENTATION_RELATIONSHIP ('NONE','NONE', #12685, #1017 ) REPRESENTATION_RELATIONSHIP_WITH_TRANSFORMATION ( #6431 )SHAPE_REPRESENTATION_RELATIONSHIP( ) );
#2715 = B_SPLINE_CURVE_WITH_KNOTS ( 'NONE', 3,
 ( #2759, #7451, #12117, #7972, #12650, #8974 ),
 .UNSPECIFIED., .F., .F.,
 ( 4, 2, 4 ),
 ( 4.462636808902389156E-07, 0.001879885123572231200, 0.003759323983463572477 ),
 .UNSPECIFIED. ) ;
#2716 = PRODUCT_DEFINITION_CONTEXT ( 'detailed design', #5486, 'design' ) ;
#2717 = PLANE ( 'NONE',  #13142 ) ;
#2718 = ORIENTED_EDGE ( 'NONE', *, *, #7125, .T. ) ;
#2719 = CARTESIAN_POINT ( 'NONE',  ( -9.403944755730119454, -4.794738323547945491, 14.99999999999999822 ) ) ;
#2720 = FACE_OUTER_BOUND ( 'NONE', #3492, .T. ) ;
#2721 = EDGE_CURVE ( 'NONE', #14061, #6410, #1776, .T. ) ;
#2722 = ADVANCED_FACE ( 'NONE', ( #6800 ), #6656, .F. ) ;
#2723 = LINE ( 'NONE', #2557, #9179 ) ;
#2724 = ORIENTED_EDGE ( 'NONE', *, *, #2527, .F. ) ;
#2725 = DIRECTION ( 'NONE',  ( -1.000000000000000000, -0.000000000000000000, -0.000000000000000000 ) ) ;
#2726 = EDGE_CURVE ( 'NONE', #11269, #13370, #10366, .T. ) ;
#2727 = CARTESIAN_POINT ( 'NONE',  ( 0.09203962824862134406, 11.73065272960076832, -9.756102650610117166 ) ) ;
#2728 = ORIENTED_EDGE ( 'NONE', *, *, #1769, .F. ) ;
#2729 = CARTESIAN_POINT ( 'NONE',  ( 0.000000000000000000, -12.98979500319698488, 5.249430348645709010 ) ) ;
#2730 = DIRECTION ( 'NONE',  ( 1.000000000000000000, 0.000000000000000000, 0.000000000000000000 ) ) ;
#2731 = EDGE_LOOP ( 'NONE', ( #3627, #2505, #5199, #13701 ) ) ;
#2732 = EDGE_LOOP ( 'NONE', ( #10242, #9798, #5877, #6411 ) ) ;
#2733 = CARTESIAN_POINT ( 'NONE',  ( 0.000000000000000000, 0.000000000000000000, 7.000000000000000000 ) ) ;
#2734 = CARTESIAN_POINT ( 'NONE',  ( 2.765633920072241736, -9.836394144775550075, -22.71065055754462492 ) ) ;
#2735 = EDGE_CURVE ( 'NONE', #1249, #1439, #13083, .T. ) ;
#2736 = CARTESIAN_POINT ( 'NONE',  ( 88.46153288930041469, 16.46030115554384565, 4.000000000000000000 ) ) ;
#2737 = CARTESIAN_POINT ( 'NONE',  ( 0.02436607992776498519, -21.30679549418621832, -12.59161484032935618 ) ) ;
#2738 = ORIENTED_EDGE ( 'NONE', *, *, #6852, .F. ) ;
#2739 = CARTESIAN_POINT ( 'NONE',  ( 1.749999999999999778, -4.835383649608602674, 17.29145405592687013 ) ) ;
#2740 = FACE_OUTER_BOUND ( 'NONE', #10000, .T. ) ;
#2741 = CYLINDRICAL_SURFACE ( 'NONE', #1701, 2.999999999999975131 ) ;
#2742 = CARTESIAN_POINT ( 'NONE',  ( 2.783068930044319433, -18.43696893154769612, 16.17493693894872564 ) ) ;
#2743 = EDGE_LOOP ( 'NONE', ( #6165, #4935, #6542, #7775 ) ) ;
#2744 = ORIENTED_EDGE ( 'NONE', *, *, #2132, .F. ) ;
#2745 = ORIENTED_EDGE ( 'NONE', *, *, #3571, .F. ) ;
#2746 = DIRECTION ( 'NONE',  ( 0.000000000000000000, 0.000000000000000000, 1.000000000000000000 ) ) ;
#2747 = DIRECTION ( 'NONE',  ( -1.000000000000000000, -0.000000000000000000, -0.000000000000000000 ) ) ;
#2748 = LINE ( 'NONE', #13340, #9757 ) ;
#2749 = DIRECTION ( 'NONE',  ( -0.000000000000000000, -0.000000000000000000, 1.000000000000000000 ) ) ;
#2750 = DIRECTION ( 'NONE',  ( 0.000000000000000000, 0.000000000000000000, 1.000000000000000000 ) ) ;
#2751 = CARTESIAN_POINT ( 'NONE',  ( 1.955869215373660985, 16.87476769693374123, 4.976600677180526233 ) ) ;
#2752 = ORIENTED_EDGE ( 'NONE', *, *, #8228, .F. ) ;
#2753 = DIRECTION ( 'NONE',  ( -1.000000000000000000, -0.000000000000000000, -0.000000000000000000 ) ) ;
#2754 = LINE ( 'NONE', #10969, #6483 ) ;
#2755 = ORIENTED_EDGE ( 'NONE', *, *, #6452, .F. ) ;
#2756 = CARTESIAN_POINT ( 'NONE',  ( 0.02436607992775544421, -22.71065055754445439, -9.836394144775947979 ) ) ;
#2757 = CIRCLE ( 'NONE', #11337, 4.000000000000000000 ) ;
#2758 = CARTESIAN_POINT ( 'NONE',  ( 2.789999999999999147, 1.991882183130294637, 24.04302995059966364 ) ) ;
#2759 = CARTESIAN_POINT ( 'NONE',  ( 1.749999999999998002, -19.67366047555545094, 20.02152543075338187 ) ) ;
#2760 = ORIENTED_EDGE ( 'NONE', *, *, #14481, .T. ) ;
#2761 = FACE_OUTER_BOUND ( 'NONE', #3674, .T. ) ;
#2762 = CYLINDRICAL_SURFACE ( 'NONE', #13643, 6.000000000000001776 ) ;
#2763 = ORIENTED_EDGE ( 'NONE', *, *, #936, .F. ) ;
#2764 = ORIENTED_EDGE ( 'NONE', *, *, #11047, .F. ) ;
#2765 = EDGE_LOOP ( 'NONE', ( #8581, #8099, #9477, #3972, #4007, #4237 ) ) ;
#2766 = FILL_AREA_STYLE ('',( #12289 ) ) ;
#2767 = DIRECTION ( 'NONE',  ( -1.000000000000000000, -0.000000000000000000, -0.000000000000000000 ) ) ;
#2768 = AXIS2_PLACEMENT_3D ( 'NONE', #14208, #5916, #4694 ) ;
#2769 = DIRECTION ( 'NONE',  ( -1.000000000000000000, -0.000000000000000000, -0.000000000000000000 ) ) ;
#2770 = DIRECTION ( 'NONE',  ( -1.000000000000000000, -0.000000000000000000, -0.000000000000000000 ) ) ;
#2771 = DIRECTION ( 'NONE',  ( 0.000000000000000000, 0.000000000000000000, 1.000000000000000000 ) ) ;
#2772 = CARTESIAN_POINT ( 'NONE',  ( 2.604434514863827488, 23.63475234378997314, -10.67816411292140444 ) ) ;
#2773 = VERTEX_POINT ( 'NONE', #11331 ) ;
#2774 = CARTESIAN_POINT ( 'NONE',  ( 0.000000000000000000, -11.04103753892277417, 8.624777288397769581 ) ) ;
#2775 = ADVANCED_FACE ( 'NONE', ( #2264 ), #10128, .T. ) ;
#2776 = EDGE_CURVE ( 'NONE', #8684, #11326, #11860, .T. ) ;
#2777 = ORIENTED_EDGE ( 'NONE', *, *, #9895, .F. ) ;
#2778 = ORIENTED_EDGE ( 'NONE', *, *, #3175, .T. ) ;
#2779 = CARTESIAN_POINT ( 'NONE',  ( 2.789999999999999147, 7.909232158575156824, -21.81711360614291806 ) ) ;
#2780 = ORIENTED_EDGE ( 'NONE', *, *, #2726, .T. ) ;
#2781 = CARTESIAN_POINT ( 'NONE',  ( 2.789999999999999147, -14.59528211760000005, -3.120158876139185189 ) ) ;
#2782 = ADVANCED_FACE ( 'NONE', ( #15032 ), #84, .T. ) ;
#2783 = ORIENTED_EDGE ( 'NONE', *, *, #612, .F. ) ;
#2784 = EDGE_CURVE ( 'NONE', #214, #4354, #1109, .T. ) ;
#2785 = CARTESIAN_POINT ( 'NONE',  ( 2.030753616560878161, -12.05220173035456632, 24.80264696524878687 ) ) ;
#2786 = CARTESIAN_POINT ( 'NONE',  ( 0.7589665283901001480, -3.797536611356509439, 27.31260702007174146 ) ) ;
#2787 = AXIS2_PLACEMENT_3D ( 'NONE', #4837, #10964, #2520 ) ;
#2788 = LINE ( 'NONE', #10855, #6478 ) ;
#2789 = CYLINDRICAL_SURFACE ( 'NONE', #1051, 4.424999999999999822 ) ;
#2790 = CYLINDRICAL_SURFACE ( 'NONE', #2128, 2.524999999999997691 ) ;
#2791 = VERTEX_POINT ( 'NONE', #6950 ) ;
#2792 = DIRECTION ( 'NONE',  ( -1.000000000000000000, -0.000000000000000000, -0.000000000000000000 ) ) ;
#2793 = CARTESIAN_POINT ( 'NONE',  ( 91.12964445316929130, 15.08873975234342701, 2.999999999999999112 ) ) ;
#2794 = CIRCLE ( 'NONE', #8938, 4.424999999999999822 ) ;
#2795 = ORIENTED_EDGE ( 'NONE', *, *, #11404, .F. ) ;
#2796 = ORIENTED_EDGE ( 'NONE', *, *, #8740, .T. ) ;
#2797 = CARTESIAN_POINT ( 'NONE',  ( -10.40394475573011945, -10.79473832354794460, 12.00000000000000000 ) ) ;
#2798 = CARTESIAN_POINT ( 'NONE',  ( 2.789999999999999147, -14.59528211760004446, 3.120158876138978687 ) ) ;
#2799 = EDGE_CURVE ( 'NONE', #5498, #1181, #8198, .T. ) ;
#2800 = CARTESIAN_POINT ( 'NONE',  ( 2.031033465052724196, 27.14933624560908498, 4.828387785248115627 ) ) ;
#2801 = AXIS2_PLACEMENT_3D ( 'NONE', #12055, #14466, #11903 ) ;
#2802 = EDGE_CURVE ( 'NONE', #12114, #8930, #826, .T. ) ;
#2803 = VECTOR ( 'NONE', #1324, 1000.000000000000000 ) ;
#2804 = LINE ( 'NONE', #14653, #2676 ) ;
#2805 = AXIS2_PLACEMENT_3D ( 'NONE', #5628, #772, #4469 ) ;
#2806 = EDGE_LOOP ( 'NONE', ( #13025, #13263, #13186, #723 ) ) ;
#2807 = DIRECTION ( 'NONE',  ( -1.000000000000000000, -0.000000000000000000, -0.000000000000000000 ) ) ;
#2808 = LINE ( 'NONE', #12175, #292 ) ;
#2809 = DIRECTION ( 'NONE',  ( -1.000000000000000000, -0.000000000000000000, -0.000000000000000000 ) ) ;
#2810 = CARTESIAN_POINT ( 'NONE',  ( 0.000000000000000000, 9.324097380959415204, 22.25075486061743391 ) ) ;
#2811 = EDGE_CURVE ( 'NONE', #7859, #7552, #11625, .T. ) ;
#2812 = VERTEX_POINT ( 'NONE', #12847 ) ;
#2813 = ORIENTED_EDGE ( 'NONE', *, *, #2248, .F. ) ;
#2814 = VECTOR ( 'NONE', #3591, 1000.000000000000000 ) ;
#2815 = VECTOR ( 'NONE', #7634, 1000.000000000000000 ) ;
#2816 = CIRCLE ( 'NONE', #93, 0.5999999999999998668 ) ;
#2817 = VERTEX_POINT ( 'NONE', #12709 ) ;
#2818 = CARTESIAN_POINT ( 'NONE',  ( 0.02436607992776411782, -24.63872515616084513, 2.336989772644183283 ) ) ;
#2819 = CARTESIAN_POINT ( 'NONE',  ( -3.510166481118844661, -1.455586230640303347, -7.800000000000008704 ) ) ;
#2820 = DIRECTION ( 'NONE',  ( -1.000000000000000000, 0.000000000000000000, 0.000000000000000000 ) ) ;
#2821 = DIRECTION ( 'NONE',  ( -1.000000000000000000, 0.000000000000000000, 0.000000000000000000 ) ) ;
#2822 = APPLICATION_PROTOCOL_DEFINITION ( 'draft international standard', 'automotive_design', 1998, #4900 ) ;
#2823 = DIRECTION ( 'NONE',  ( 0.1305261922200521840, -0.9914448613738103822, 0.000000000000000000 ) ) ;
#2824 = PRODUCT ( 'MAS-167', 'MAS-167', '', ( #12273 ) ) ;
#2825 = VERTEX_POINT ( 'NONE', #8481 ) ;
#2826 = CARTESIAN_POINT ( 'NONE',  ( -14.40394475573011945, -10.79473832354794460, -3.469446951953614189E-15 ) ) ;
#2827 = FACE_OUTER_BOUND ( 'NONE', #8620, .T. ) ;
#2828 = ORIENTED_EDGE ( 'NONE', *, *, #8518, .F. ) ;
#2829 = CARTESIAN_POINT ( 'NONE',  ( 1.749999999999998002, -12.96210679857804671, 24.89775460606827551 ) ) ;
#2830 = CARTESIAN_POINT ( 'NONE',  ( 1.039999999999995817, 4.633866840648921404, 27.68468304288260029 ) ) ;
#2831 = CIRCLE ( 'NONE', #4804, 5.999999999999999112 ) ;
#2832 = CARTESIAN_POINT ( 'NONE',  ( 1.039999999999996039, 19.67366047555559305, -20.02152543075323976 ) ) ;
#2833 = ADVANCED_FACE ( 'NONE', ( #7022 ), #8246, .F. ) ;
#2834 = ORIENTED_EDGE ( 'NONE', *, *, #10095, .F. ) ;
#2835 = DIRECTION ( 'NONE',  ( 0.5416238976136762417, -0.8406209333187996124, 0.000000000000000000 ) ) ;
#2836 = CARTESIAN_POINT ( 'NONE',  ( 2.764680872513688659, 2.311161484776556030, 14.46287784598618309 ) ) ;
#2837 = EDGE_LOOP ( 'NONE', ( #14020, #12866, #11290, #13398 ) ) ;
#2838 = ORIENTED_EDGE ( 'NONE', *, *, #5024, .F. ) ;
#2839 = CYLINDRICAL_SURFACE ( 'NONE', #2380, 3.799999999999999378 ) ;
#2840 = CIRCLE ( 'NONE', #104, 28.06981291497571007 ) ;
#2841 = DIRECTION ( 'NONE',  ( -1.000000000000000000, -0.000000000000000000, -0.000000000000000000 ) ) ;
#2842 = CARTESIAN_POINT ( 'NONE',  ( 0.4522159373304736607, -16.32199768300077380, -3.429166897524598134 ) ) ;
#2843 = DIRECTION ( 'NONE',  ( 0.000000000000000000, -1.000000000000000000, 0.000000000000000000 ) ) ;
#2844 = DIRECTION ( 'NONE',  ( 5.339417856040273846E-17, 1.063174570779084847E-17, -1.000000000000000000 ) ) ;
#2845 = DIRECTION ( 'NONE',  ( -1.000000000000000000, 0.000000000000000000, -0.000000000000000000 ) ) ;
#2846 = B_SPLINE_CURVE_WITH_KNOTS ( 'NONE', 3,
 ( #4313, #14926, #10304, #13763 ),
 .UNSPECIFIED., .F., .F.,
 ( 4, 4 ),
 ( 2.159563976582245544E-07, 0.0006916893629248793826 ),
 .UNSPECIFIED. ) ;
#2847 = EDGE_CURVE ( 'NONE', #8589, #5623, #4685, .T. ) ;
#2848 = ORIENTED_EDGE ( 'NONE', *, *, #8770, .T. ) ;
#2849 = DIRECTION ( 'NONE',  ( 0.000000000000000000, 0.000000000000000000, 1.000000000000000000 ) ) ;
#2850 = B_SPLINE_CURVE_WITH_KNOTS ( 'NONE', 3,
 ( #12608, #5642, #12686, #11380 ),
 .UNSPECIFIED., .F., .F.,
 ( 4, 4 ),
 ( 0.005123695899043908056, 0.005814329666474866640 ),
 .UNSPECIFIED. ) ;
#2851 = B_SPLINE_CURVE_WITH_KNOTS ( 'NONE', 3,
 ( #1630, #5335, #12229, #10004 ),
 .UNSPECIFIED., .F., .F.,
 ( 4, 4 ),
 ( 0.005258105385878670927, 0.005948373736081390140 ),
 .UNSPECIFIED. ) ;
#2852 = ORIENTED_EDGE ( 'NONE', *, *, #3382, .F. ) ;
#2853 = VERTEX_POINT ( 'NONE', #5884 ) ;
#2854 = EDGE_LOOP ( 'NONE', ( #9779, #14271, #2653, #12124 ) ) ;
#2855 = DIRECTION ( 'NONE',  ( 0.000000000000000000, 0.000000000000000000, 1.000000000000000000 ) ) ;
#2856 = ADVANCED_FACE ( 'NONE', ( #15106 ), #4500, .T. ) ;
#2857 = TOROIDAL_SURFACE ( 'NONE', #5337, 24.12539914357697768, 8.000000000000000000 ) ;
#2858 = ORIENTED_EDGE ( 'NONE', *, *, #5653, .T. ) ;
#2859 = CIRCLE ( 'NONE', #10946, 5.575000000000000178 ) ;
#2860 = EDGE_CURVE ( 'NONE', #11203, #4549, #10404, .T. ) ;
#2861 = PRODUCT_DEFINITION_CONTEXT ( 'detailed design', #4900, 'design' ) ;
#2862 = AXIS2_PLACEMENT_3D ( 'NONE', #7345, #3955, #5268 ) ;
#2863 = FACE_OUTER_BOUND ( 'NONE', #10289, .T. ) ;
#2864 = ORIENTED_EDGE ( 'NONE', *, *, #10013, .F. ) ;
#2865 = CARTESIAN_POINT ( 'NONE',  ( -5.209999999999999964, 0.000000000000000000, 0.000000000000000000 ) ) ;
#2866 = DIRECTION ( 'NONE',  ( -1.000000000000000000, -0.000000000000000000, -0.000000000000000000 ) ) ;
#2867 = CARTESIAN_POINT ( 'NONE',  ( 1.749999999999999778, 12.83329210556849453, -12.55714665599973578 ) ) ;
#2868 = DIRECTION ( 'NONE',  ( 0.000000000000000000, 0.000000000000000000, 1.000000000000000000 ) ) ;
#2869 = B_SPLINE_CURVE_WITH_KNOTS ( 'NONE', 3,
 ( #10220, #5473, #5547, #13598, #9075, #11298 ),
 .UNSPECIFIED., .F., .F.,
 ( 4, 2, 4 ),
 ( 1.979325885420462316E-07, 0.001878588715165608420, 0.003756979497742674902 ),
 .UNSPECIFIED. ) ;
#2870 = CARTESIAN_POINT ( 'NONE',  ( 1.039999999999997815, 27.68468304288265003, -4.633866840648637186 ) ) ;
#2871 = EDGE_LOOP ( 'NONE', ( #3029, #1463, #9846, #14579 ) ) ;
#2872 = AXIS2_PLACEMENT_3D ( 'NONE', #1358, #14205, #14123 ) ;
#2873 = CARTESIAN_POINT ( 'NONE',  ( 0.008751532932800723183, 13.40591150984233870, -5.214906618939568084 ) ) ;
#2874 = EDGE_CURVE ( 'NONE', #2548, #11986, #2194, .T. ) ;
#2875 = CARTESIAN_POINT ( 'NONE',  ( 1.394999999999998685, 12.55714665600005375, -12.83329210556818722 ) ) ;
#2876 = TOROIDAL_SURFACE ( 'NONE', #2146, 14.01039946648074341, 8.000000000000000000 ) ;
#2877 = ORIENTED_EDGE ( 'NONE', *, *, #4223, .T. ) ;
#2878 = ORIENTED_EDGE ( 'NONE', *, *, #6158, .T. ) ;
#2879 = CYLINDRICAL_SURFACE ( 'NONE', #9523, 2.999999999999988898 ) ;
#2880 = DIRECTION ( 'NONE',  ( 0.6743761619433820131, 0.7383879686198261405, -5.947623346206184252E-19 ) ) ;
#2881 = CIRCLE ( 'NONE', #12200, 4.000000000000000000 ) ;
#2882 =( NAMED_UNIT ( * ) SI_UNIT ( $, .STERADIAN. ) SOLID_ANGLE_UNIT ( ) );
#2883 = DIRECTION ( 'NONE',  ( 0.000000000000000000, 0.000000000000000000, 1.000000000000000000 ) ) ;
#2884 = EDGE_CURVE ( 'NONE', #12893, #13854, #12925, .T. ) ;
#2885 = AXIS2_PLACEMENT_3D ( 'NONE', #14830, #4299, #6831 ) ;
#2886 = DIRECTION ( 'NONE',  ( 1.576560579138138762E-17, -1.359337748750801608E-17, 1.000000000000000000 ) ) ;
#2887 =( GEOMETRIC_REPRESENTATION_CONTEXT ( 3 ) GLOBAL_UNCERTAINTY_ASSIGNED_CONTEXT ( ( #8762 ) ) GLOBAL_UNIT_ASSIGNED_CONTEXT ( ( #5206, #8711, #2882 ) ) REPRESENTATION_CONTEXT ( 'NONE', 'WORKASPACE' ) );
#2888 = ORIENTED_EDGE ( 'NONE', *, *, #5568, .T. ) ;
#2889 = DIRECTION ( 'NONE',  ( 0.000000000000000000, 0.000000000000000000, 1.000000000000000000 ) ) ;
#2890 = DIRECTION ( 'NONE',  ( -0.000000000000000000, 1.000000000000000000, 0.000000000000000000 ) ) ;
#2891 = AXIS2_PLACEMENT_3D ( 'NONE', #12339, #14440, #424 ) ;
#2892 = VECTOR ( 'NONE', #14504, 1000.000000000000000 ) ;
#2893 = DIRECTION ( 'NONE',  ( -1.000000000000000000, 0.000000000000000000, 0.000000000000000000 ) ) ;
#2894 = CARTESIAN_POINT ( 'NONE',  ( 2.765633920072238183, -18.55949924794904504, 16.37294372382852004 ) ) ;
#2895 = VERTEX_POINT ( 'NONE', #2416 ) ;
#2896 = ORIENTED_EDGE ( 'NONE', *, *, #14272, .T. ) ;
#2897 = ADVANCED_FACE ( 'NONE', ( #11779 ), #1256, .F. ) ;
#2898 = EDGE_CURVE ( 'NONE', #10516, #15169, #13842, .T. ) ;
#2899 = ORIENTED_EDGE ( 'NONE', *, *, #5713, .T. ) ;
#2900 = AXIS2_PLACEMENT_3D ( 'NONE', #9533, #14382, #8301 ) ;
#2901 = CARTESIAN_POINT ( 'NONE',  ( 2.765633920072238183, 2.336989772644269436, 24.63872515616083447 ) ) ;
#2902 = DIRECTION ( 'NONE',  ( -0.000000000000000000, -1.000000000000000000, -0.000000000000000000 ) ) ;
#2903 = VECTOR ( 'NONE', #3984, 1000.000000000000000 ) ;
#2904 = DIRECTION ( 'NONE',  ( -0.000000000000000000, -0.000000000000000000, 1.000000000000000000 ) ) ;
#2905 = CARTESIAN_POINT ( 'NONE',  ( -5.209999999999999964, 0.000000000000000000, 0.000000000000000000 ) ) ;
#2906 = PRODUCT_CONTEXT ( 'NONE', #2917, 'mechanical' ) ;
#2907 = DIRECTION ( 'NONE',  ( 0.000000000000000000, 0.000000000000000000, 1.000000000000000000 ) ) ;
#2908 = LINE ( 'NONE', #11048, #977 ) ;
#2909 = DIRECTION ( 'NONE',  ( -1.000000000000000000, -0.000000000000000000, -0.000000000000000000 ) ) ;
#2910 = ORIENTED_EDGE ( 'NONE', *, *, #3691, .T. ) ;
#2911 = CARTESIAN_POINT ( 'NONE',  ( 2.789999999999999147, -8.624777288397723396, -11.04103753892280615 ) ) ;
#2912 = DIRECTION ( 'NONE',  ( 0.000000000000000000, 0.000000000000000000, 1.000000000000000000 ) ) ;
#2913 = EDGE_CURVE ( 'NONE', #8078, #6064, #6238, .T. ) ;
#2914 = CARTESIAN_POINT ( 'NONE',  ( 1.039999999999995373, -12.96210679857767900, -24.89775460606846380 ) ) ;
#2915 = EDGE_CURVE ( 'NONE', #13200, #4678, #7219, .T. ) ;
#2916 = ORIENTED_EDGE ( 'NONE', *, *, #163, .T. ) ;
#2917 = APPLICATION_CONTEXT ( 'automotive_design' ) ;
#2918 = AXIS2_PLACEMENT_3D ( 'NONE', #11500, #15210, #6043 ) ;
#2919 = ADVANCED_FACE ( 'NONE', ( #9558 ), #1851, .F. ) ;
#2920 = CARTESIAN_POINT ( 'NONE',  ( -4.000000000000000000, 0.000000000000000000, 4.500000000000000888 ) ) ;
#2921 = CARTESIAN_POINT ( 'NONE',  ( 2.789999999999999147, 1.621424371464993087E-13, -15.47981323787947794 ) ) ;
#2922 = EDGE_LOOP ( 'NONE', ( #11069, #10023, #658, #4273, #10697, #2464 ) ) ;
#2923 = ORIENTED_EDGE ( 'NONE', *, *, #6352, .F. ) ;
#2924 = CARTESIAN_POINT ( 'NONE',  ( 2.789999999999999147, -9.514945144208585504, -22.37986894186682107 ) ) ;
#2925 = CARTESIAN_POINT ( 'NONE',  ( 0.000000000000000000, -7.739906618939614624, -13.40591150984234581 ) ) ;
#2926 = DIRECTION ( 'NONE',  ( 0.000000000000000000, 0.000000000000000000, 1.000000000000000000 ) ) ;
#2927 = FACE_OUTER_BOUND ( 'NONE', #11823, .T. ) ;
#2928 = LINE ( 'NONE', #9607, #7239 ) ;
#2929 = EDGE_CURVE ( 'NONE', #134, #2475, #2558, .T. ) ;
#2930 = CARTESIAN_POINT ( 'NONE',  ( 64.00448238961524794, 36.25062540154047497, 5.000000000000000888 ) ) ;
#2931 = VECTOR ( 'NONE', #1289, 1000.000000000000000 ) ;
#2932 = AXIS2_PLACEMENT_3D ( 'NONE', #1185, #13241, #3781 ) ;
#2933 = VECTOR ( 'NONE', #3430, 1000.000000000000000 ) ;
#2934 = VERTEX_POINT ( 'NONE', #4085 ) ;
#2935 = CARTESIAN_POINT ( 'NONE',  ( 2.262072625383134916, -26.57710921259758408, -4.996265754456650221 ) ) ;
#2936 = EDGE_LOOP ( 'NONE', ( #9229, #2778, #1228, #8215 ) ) ;
#2937 = EDGE_LOOP ( 'NONE', ( #11951, #5390, #3768, #9077, #3420, #14158, #8321, #10483 ) ) ;
#2938 = ORIENTED_EDGE ( 'NONE', *, *, #2248, .T. ) ;
#2939 = AXIS2_PLACEMENT_3D ( 'NONE', #3535, #12830, #11606 ) ;
#2940 = CARTESIAN_POINT ( 'NONE',  ( 2.790000000000010694, -14.05347802000170354, 2.096460570596122341 ) ) ;
#2941 = CARTESIAN_POINT ( 'NONE',  ( 2.718184757033982546, 16.91181672897760535, -18.89296398180173497 ) ) ;
#2942 = CARTESIAN_POINT ( 'NONE',  ( 19.20634328910001543, -26.21503864878155099, -2.000000000000000000 ) ) ;
#2943 = DIRECTION ( 'NONE',  ( -0.000000000000000000, -0.000000000000000000, 1.000000000000000000 ) ) ;
#2944 = ORIENTED_EDGE ( 'NONE', *, *, #6661, .F. ) ;
#2945 = CARTESIAN_POINT ( 'NONE',  ( 0.08915872821341043475, 14.29252738795465483, 5.279841123860395058 ) ) ;
#2946 = CARTESIAN_POINT ( 'NONE',  ( -5.209999999999999964, 0.000000000000000000, 0.000000000000000000 ) ) ;
#2947 = AXIS2_PLACEMENT_3D ( 'NONE', #12814, #1288, #9302 ) ;
#2948 = FACE_OUTER_BOUND ( 'NONE', #10756, .T. ) ;
#2949 = CARTESIAN_POINT ( 'NONE',  ( 84.00000000000000000, 0.000000000000000000, 4.000000000000003553 ) ) ;
#2950 = EDGE_CURVE ( 'NONE', #4042, #11203, #2551, .T. ) ;
#2951 = CARTESIAN_POINT ( 'NONE',  ( 0.000000000000000000, -18.28042085475288303, 15.74360496233377305 ) ) ;
#2952 = ORIENTED_EDGE ( 'NONE', *, *, #6015, .F. ) ;
#2953 = CARTESIAN_POINT ( 'NONE',  ( 0.1085714285714285687, -3.798448662927795372, -0.8000000000000000444 ) ) ;
#2954 = PRODUCT_DEFINITION_SHAPE ( 'NONE', 'NONE',  #12277 ) ;
#2955 = CARTESIAN_POINT ( 'NONE',  ( 3.510166481118872639, 1.455586230640303791, -7.000000000000007994 ) ) ;
#2956 = ORIENTED_EDGE ( 'NONE', *, *, #14767, .T. ) ;
#2957 = VERTEX_POINT ( 'NONE', #3708 ) ;
#2958 = DIRECTION ( 'NONE',  ( 1.000000000000000000, 0.000000000000000000, 0.000000000000000000 ) ) ;
#2959 = DIRECTION ( 'NONE',  ( -1.000000000000000000, 0.000000000000000000, 0.000000000000000000 ) ) ;
#2960 = FACE_BOUND ( 'NONE', #10830, .T. ) ;
#2961 = CARTESIAN_POINT ( 'NONE',  ( 2.782672435525938237, -9.044896821682277377, 11.23174270417326071 ) ) ;
#2962 = ORIENTED_EDGE ( 'NONE', *, *, #13779, .T. ) ;
#2963 = DIRECTION ( 'NONE',  ( -1.000000000000000000, 0.000000000000000000, 0.000000000000000000 ) ) ;
#2964 = CARTESIAN_POINT ( 'NONE',  ( 59.43001430450886602, 34.23215029930534570, 5.000000000000000888 ) ) ;
#2965 = ORIENTED_EDGE ( 'NONE', *, *, #10146, .T. ) ;
#2966 = CARTESIAN_POINT ( 'NONE',  ( -11.52599798030746037, -13.27615371759915242, 0.7999999999999959366 ) ) ;
#2967 = EDGE_CURVE ( 'NONE', #11474, #10155, #7711, .T. ) ;
#2968 = ORIENTED_EDGE ( 'NONE', *, *, #14230, .F. ) ;
#2969 = ORIENTED_EDGE ( 'NONE', *, *, #2776, .F. ) ;
#2970 = EDGE_CURVE ( 'NONE', #2441, #9761, #14339, .T. ) ;
#2971 = VERTEX_POINT ( 'NONE', #6460 ) ;
#2972 = DIRECTION ( 'NONE',  ( 0.1643989873053574302, -0.9863939238321437486, 0.000000000000000000 ) ) ;
#2973 = CARTESIAN_POINT ( 'NONE',  ( 0.02436607992775934733, -2.336989772644440855, 24.63872515616082026 ) ) ;
#2974 = CARTESIAN_POINT ( 'NONE',  ( -16.14082873121598993, -7.414910804916202913, -3.000000000000000000 ) ) ;
#2975 = DIRECTION ( 'NONE',  ( 0.000000000000000000, 0.000000000000000000, 1.000000000000000000 ) ) ;
#2976 = SHAPE_DEFINITION_REPRESENTATION ( #5300, #10044 ) ;
#2977 = CARTESIAN_POINT ( 'NONE',  ( 0.02531912748679129854, -9.232963481057844035, 11.36963888406684298 ) ) ;
#2978 = PLANE ( 'NONE',  #14489 ) ;
#2979 = CARTESIAN_POINT ( 'NONE',  ( 2.789999999999999147, -14.18181402625728360, -19.91106274590529068 ) ) ;
#2980 = ADVANCED_FACE ( 'NONE', ( #3004 ), #1774, .F. ) ;
#2981 = ORIENTED_EDGE ( 'NONE', *, *, #10353, .T. ) ;
#2982 = FACE_OUTER_BOUND ( 'NONE', #3019, .T. ) ;
#2983 = EDGE_CURVE ( 'NONE', #6106, #14255, #4870, .T. ) ;
#2984 = CARTESIAN_POINT ( 'NONE',  ( 2.789999999999999147, 23.31896751603342821, -7.334849878007252855 ) ) ;
#2985 = AXIS2_PLACEMENT_3D ( 'NONE', #7936, #1793, #6705 ) ;
#2986 = CARTESIAN_POINT ( 'NONE',  ( 80.00000000000000000, -9.999999999999994671, 3.000000000000002665 ) ) ;
#2987 = ORIENTED_EDGE ( 'NONE', *, *, #2970, .T. ) ;
#2988 = CARTESIAN_POINT ( 'NONE',  ( -19.40394475573012301, -7.794738323547950820, 14.99999999999999822 ) ) ;
#2989 = CYLINDRICAL_SURFACE ( 'NONE', #12160, 13.19999999999999929 ) ;
#2990 = EDGE_LOOP ( 'NONE', ( #6073, #12287, #2136, #1334, #14701, #11260, #2012, #5617 ) ) ;
#2991 = VERTEX_POINT ( 'NONE', #11137 ) ;
#2992 = CARTESIAN_POINT ( 'NONE',  ( 6.000000000000000888, 0.000000000000000000, 4.500000000000000888 ) ) ;
#2993 = CARTESIAN_POINT ( 'NONE',  ( 2.789999999999999147, 5.249430348645756084, 12.98979500319695823 ) ) ;
#2994 = DIRECTION ( 'NONE',  ( 1.000000000000000000, 0.000000000000000000, 0.000000000000000000 ) ) ;
#2995 = DIRECTION ( 'NONE',  ( 0.000000000000000000, 0.000000000000000000, 1.000000000000000000 ) ) ;
#2996 = EDGE_CURVE ( 'NONE', #4663, #418, #6389, .T. ) ;
#2997 = DIRECTION ( 'NONE',  ( -1.000000000000000000, -0.000000000000000000, -0.000000000000000000 ) ) ;
#2998 = EDGE_CURVE ( 'NONE', #4961, #5235, #11224, .T. ) ;
#2999 = CARTESIAN_POINT ( 'NONE',  ( 0.7589665326895889130, -12.98167595241004335, -24.32849926382764849 ) ) ;
#3000 = DIRECTION ( 'NONE',  ( 0.000000000000000000, 0.000000000000000000, -1.000000000000000000 ) ) ;
#3001 = EDGE_CURVE ( 'NONE', #4926, #10057, #13355, .T. ) ;
#3002 = ORIENTED_EDGE ( 'NONE', *, *, #6852, .T. ) ;
#3003 = DIRECTION ( 'NONE',  ( -1.000000000000000000, 0.000000000000000000, 0.000000000000000000 ) ) ;
#3004 = FACE_OUTER_BOUND ( 'NONE', #3852, .T. ) ;
#3005 = ORIENTED_EDGE ( 'NONE', *, *, #2409, .F. ) ;
#3006 = EDGE_CURVE ( 'NONE', #13883, #14059, #13088, .T. ) ;
#3007 = B_SPLINE_CURVE_WITH_KNOTS ( 'NONE', 3,
 ( #12550, #2025, #2324, #13934 ),
 .UNSPECIFIED., .F., .F.,
 ( 4, 4 ),
 ( 2.135345996541640089E-07, 0.0006888010880211291841 ),
 .UNSPECIFIED. ) ;
#3008 = CIRCLE ( 'NONE', #11105, 14.01039946648073986 ) ;
#3009 = AXIS2_PLACEMENT_3D ( 'NONE', #6497, #8950, #2036 ) ;
#3010 = VERTEX_POINT ( 'NONE', #5408 ) ;
#3011 = ORIENTED_EDGE ( 'NONE', *, *, #980, .T. ) ;
#3012 = ORIENTED_EDGE ( 'NONE', *, *, #7407, .F. ) ;
#3013 = DIRECTION ( 'NONE',  ( 0.7573544145849105957, -0.6530040510661073716, -2.853163611803960010E-17 ) ) ;
#3014 = LINE ( 'NONE', #14482, #6999 ) ;
#3015 = UNCERTAINTY_MEASURE_WITH_UNIT (LENGTH_MEASURE( 1.000000000000000082E-05 ), #3755, 'distance_accuracy_value', 'NONE');
#3016 = LINE ( 'NONE', #2942, #5641 ) ;
#3017 = DIRECTION ( 'NONE',  ( 0.000000000000000000, 0.000000000000000000, 1.000000000000000000 ) ) ;
#3018 = B_SPLINE_CURVE_WITH_KNOTS ( 'NONE', 3,
 ( #15137, #7201, #41, #2516, #12878, #2364, #7056, #9426 ),
 .UNSPECIFIED., .F., .F.,
 ( 4, 2, 2, 4 ),
 ( 2.445728210258510103E-07, 0.001895260649874684405, 0.002842768688401516204, 0.003790276726928348220 ),
 .UNSPECIFIED. ) ;
#3019 = EDGE_LOOP ( 'NONE', ( #3012, #7526, #11091, #2728 ) ) ;
#3020 = CIRCLE ( 'NONE', #10140, 3.000000000000000888 ) ;
#3021 = DIRECTION ( 'NONE',  ( -1.000000000000000000, -0.000000000000000000, -0.000000000000000000 ) ) ;
#3022 = DIRECTION ( 'NONE',  ( 0.000000000000000000, 0.000000000000000000, 1.000000000000000000 ) ) ;
#3023 = CARTESIAN_POINT ( 'NONE',  ( 32.66827876307085887, -1.833751565556681173, 2.999999999999999112 ) ) ;
#3024 = CARTESIAN_POINT ( 'NONE',  ( 98.48580539929344013, 0.9022481406819604643, 6.000000000000000000 ) ) ;
#3025 = ORIENTED_EDGE ( 'NONE', *, *, #3209, .T. ) ;
#3026 = CARTESIAN_POINT ( 'NONE',  ( 0.02531912748464587928, -5.229914364928447412, 13.68080036884346917 ) ) ;
#3027 = CARTESIAN_POINT ( 'NONE',  ( 2.508169719062756986, -12.18203740414259606, -10.58084377126636078 ) ) ;
#3028 = EDGE_LOOP ( 'NONE', ( #10679, #15182, #11673, #9697 ) ) ;
#3029 = ORIENTED_EDGE ( 'NONE', *, *, #8709, .F. ) ;
#3030 = CARTESIAN_POINT ( 'NONE',  ( 88.46153288930041469, 16.46030115554384565, 7.000000000000000000 ) ) ;
#3031 = PRESENTATION_STYLE_ASSIGNMENT (( #7803 ) ) ;
#3032 = CARTESIAN_POINT ( 'NONE',  ( 0.000000000000000000, 25.59481291497571220, 0.000000000000000000 ) ) ;
#3033 = ORIENTED_EDGE ( 'NONE', *, *, #5415, .T. ) ;
#3034 = B_SPLINE_CURVE_WITH_KNOTS ( 'NONE', 3,
 ( #5382, #9970, #11114, #11415 ),
 .UNSPECIFIED., .F., .F.,
 ( 4, 4 ),
 ( 2.135345996175604595E-07, 0.0006888010880210905865 ),
 .UNSPECIFIED. ) ;
#3035 = DIRECTION ( 'NONE',  ( 0.000000000000000000, 1.000000000000000000, -1.084202172485504187E-16 ) ) ;
#3036 = EDGE_CURVE ( 'NONE', #4328, #4113, #10076, .T. ) ;
#3037 = ORIENTED_EDGE ( 'NONE', *, *, #10499, .T. ) ;
#3038 = DIRECTION ( 'NONE',  ( 0.4036950204470263204, -0.9148936170212770280, 0.000000000000000000 ) ) ;
#3039 = CARTESIAN_POINT ( 'NONE',  ( 50.00050000000000239, 0.000000000000000000, 0.000000000000000000 ) ) ;
#3040 = ORIENTED_EDGE ( 'NONE', *, *, #2967, .T. ) ;
#3041 = DIRECTION ( 'NONE',  ( 0.5416238976136762417, -0.8406209333187997235, -0.000000000000000000 ) ) ;
#3042 = DIRECTION ( 'NONE',  ( -1.000000000000000000, -0.000000000000000000, 0.000000000000000000 ) ) ;
#3043 = EDGE_LOOP ( 'NONE', ( #248, #14283, #9269, #1352 ) ) ;
#3044 = VERTEX_POINT ( 'NONE', #8916 ) ;
#3045 = ORIENTED_EDGE ( 'NONE', *, *, #8959, .F. ) ;
#3046 = FACE_OUTER_BOUND ( 'NONE', #4669, .T. ) ;
#3047 = CARTESIAN_POINT ( 'NONE',  ( 2.765633920072235963, 22.71065055754452544, 9.836394144775786330 ) ) ;
#3048 = ADVANCED_FACE ( 'NONE', ( #13603 ), #3085, .F. ) ;
#3049 = AXIS2_PLACEMENT_3D ( 'NONE', #6022, #8390, #10709 ) ;
#3050 = CARTESIAN_POINT ( 'NONE',  ( 1.749999999999998002, -20.02152543075331081, -19.67366047555553266 ) ) ;
#3051 = AXIS2_PLACEMENT_3D ( 'NONE', #4167, #9628, #4886 ) ;
#3052 = CARTESIAN_POINT ( 'NONE',  ( 2.789999999999999147, 16.37294372382858398, 18.55949924794898465 ) ) ;
#3053 = APPLICATION_PROTOCOL_DEFINITION ( 'draft international standard', 'automotive_design', 1998, #7547 ) ;
#3054 = DIRECTION ( 'NONE',  ( 1.000000000000000000, 0.000000000000000000, 0.000000000000000000 ) ) ;
#3055 = ADVANCED_FACE ( 'NONE', ( #166 ), #333, .T. ) ;
#3056 = AXIS2_PLACEMENT_3D ( 'NONE', #5225, #13347, #3748 ) ;
#3057 = CARTESIAN_POINT ( 'NONE',  ( -1.000000000000000000, -5.408326913195983465, -0.8000000000000000444 ) ) ;
#3058 = CARTESIAN_POINT ( 'NONE',  ( 2.789999999999999147, -23.17675759782035172, -7.772527002114682837 ) ) ;
#3059 = ORIENTED_EDGE ( 'NONE', *, *, #14913, .F. ) ;
#3060 = CARTESIAN_POINT ( 'NONE',  ( 2.781248467067199748, -13.40591150984217705, -5.214906618939849636 ) ) ;
#3061 = DIRECTION ( 'NONE',  ( -1.000000000000000000, -0.000000000000000000, -0.000000000000000000 ) ) ;
#3062 = EDGE_CURVE ( 'NONE', #11582, #4228, #68, .T. ) ;
#3063 = TOROIDAL_SURFACE ( 'NONE', #6730, 24.12539914357697413, 8.000000000000000000 ) ;
#3064 = DIRECTION ( 'NONE',  ( 0.000000000000000000, 0.000000000000000000, -1.000000000000000000 ) ) ;
#3065 = EDGE_LOOP ( 'NONE', ( #3423, #10026, #12566, #13144, #8333, #3269 ) ) ;
#3066 = AXIS2_PLACEMENT_3D ( 'NONE', #14467, #3933, #12294 ) ;
#3067 = CARTESIAN_POINT ( 'NONE',  ( 1.149999999999998135, 5.021051876504148371E-16, 4.100000000000000533 ) ) ;
#3068 = CARTESIAN_POINT ( 'NONE',  ( -19.40394475573012301, -7.794738323547950820, 14.99999999999999822 ) ) ;
#3069 = VERTEX_POINT ( 'NONE', #13686 ) ;
#3070 = ORIENTED_EDGE ( 'NONE', *, *, #7425, .T. ) ;
#3071 = DIRECTION ( 'NONE',  ( 1.000000000000000000, 0.000000000000000000, 0.000000000000000000 ) ) ;
#3072 = DIRECTION ( 'NONE',  ( 1.000000000000000000, 0.000000000000000000, 0.000000000000000000 ) ) ;
#3073 = EDGE_CURVE ( 'NONE', #555, #6387, #3306, .T. ) ;
#3074 = CARTESIAN_POINT ( 'NONE',  ( 101.4858053992934401, 0.9022481406819604643, 6.000000000000000000 ) ) ;
#3075 = CARTESIAN_POINT ( 'NONE',  ( 2.790000000000009805, 2.096460570596172968, 14.05347802000169644 ) ) ;
#3076 = CARTESIAN_POINT ( 'NONE',  ( 2.789999999999999147, -1.991882183130462503, 24.04302995059964942 ) ) ;
#3077 = VECTOR ( 'NONE', #6509, 999.9999999999998863 ) ;
#3078 = VECTOR ( 'NONE', #8387, 1000.000000000000000 ) ;
#3079 = AXIS2_PLACEMENT_3D ( 'NONE', #11309, #10083, #12306 ) ;
#3080 = DIRECTION ( 'NONE',  ( -1.000000000000000000, 0.000000000000000000, -0.000000000000000000 ) ) ;
#3081 = CARTESIAN_POINT ( 'NONE',  ( 0.000000000000000000, -8.624777288397730501, -11.04103753892280615 ) ) ;
#3082 = ORIENTED_EDGE ( 'NONE', *, *, #13303, .T. ) ;
#3083 = CARTESIAN_POINT ( 'NONE',  ( 1.039999999999995373, 25.12109765559670649, -12.52377138324197681 ) ) ;
#3084 = EDGE_CURVE ( 'NONE', #4197, #6222, #2846, .T. ) ;
#3085 = CYLINDRICAL_SURFACE ( 'NONE', #9180, 6.000000000000000888 ) ;
#3086 = ORIENTED_EDGE ( 'NONE', *, *, #9173, .T. ) ;
#3087 = CIRCLE ( 'NONE', #14127, 5.899999999999999467 ) ;
#3088 = EDGE_CURVE ( 'NONE', #8921, #6027, #9671, .T. ) ;
#3089 =( NAMED_UNIT ( * ) SI_UNIT ( $, .STERADIAN. ) SOLID_ANGLE_UNIT ( ) );
#3090 = CIRCLE ( 'NONE', #7006, 24.12539914357697768 ) ;
#3091 = ORIENTED_EDGE ( 'NONE', *, *, #344, .T. ) ;
#3092 = ORIENTED_EDGE ( 'NONE', *, *, #1734, .T. ) ;
#3093 = ORIENTED_EDGE ( 'NONE', *, *, #211, .F. ) ;
#3094 = DIRECTION ( 'NONE',  ( 1.000000000000000000, 0.000000000000000000, 0.000000000000000000 ) ) ;
#3095 = EDGE_CURVE ( 'NONE', #13251, #13045, #2077, .T. ) ;
#3096 = FILL_AREA_STYLE_COLOUR ( '', #14621 ) ;
#3097 = EDGE_CURVE ( 'NONE', #9387, #12669, #1936, .T. ) ;
#3098 = CARTESIAN_POINT ( 'NONE',  ( 58.14665764790533586, -0.9105996816177489572, 6.000000000000000000 ) ) ;
#3099 = CARTESIAN_POINT ( 'NONE',  ( -5.209999999999999964, 0.000000000000000000, 0.000000000000000000 ) ) ;
#3100 = AXIS2_PLACEMENT_3D ( 'NONE', #5086, #10980, #12048 ) ;
#3101 = VERTEX_POINT ( 'NONE', #3238 ) ;
#3102 = CARTESIAN_POINT ( 'NONE',  ( 2.257825491203655055, -11.58891744060124473, 24.44564404695840665 ) ) ;
#3103 = DIRECTION ( 'NONE',  ( -1.000000000000000000, 0.000000000000000000, 0.000000000000000000 ) ) ;
#3104 = CARTESIAN_POINT ( 'NONE',  ( 86.17559721729969624, 12.01344854909570259, 4.000000000000000000 ) ) ;
#3105 = LINE ( 'NONE', #5648, #13811 ) ;
#3106 = VECTOR ( 'NONE', #10371, 1000.000000000000000 ) ;
#3107 = VERTEX_POINT ( 'NONE', #923 ) ;
#3108 = CARTESIAN_POINT ( 'NONE',  ( 93.34550147531103903, 3.654933296868752457, -2.000000000000000888 ) ) ;
#3109 = AXIS2_PLACEMENT_3D ( 'NONE', #10354, #2137, #13747 ) ;
#3110 = DIRECTION ( 'NONE',  ( -1.000000000000000000, 0.000000000000000000, 0.000000000000000000 ) ) ;
#3111 = EDGE_CURVE ( 'NONE', #10457, #12375, #5519, .T. ) ;
#3112 = ORIENTED_EDGE ( 'NONE', *, *, #4796, .T. ) ;
#3113 = ORIENTED_EDGE ( 'NONE', *, *, #10497, .T. ) ;
#3114 = CARTESIAN_POINT ( 'NONE',  ( 8.000000000000000000, 0.000000000000000000, 0.000000000000000000 ) ) ;
#3115 = LINE ( 'NONE', #11325, #7987 ) ;
#3116 = EDGE_CURVE ( 'NONE', #3736, #546, #9425, .T. ) ;
#3117 = ORIENTED_EDGE ( 'NONE', *, *, #3440, .F. ) ;
#3118=STYLED_ITEM('',(#15286),#3717);
#3119 = CIRCLE ( 'NONE', #8498, 2.524999999999998135 ) ;
#3120 = DIRECTION ( 'NONE',  ( -5.480158469902919838E-17, -1.051478716308701618E-16, -1.000000000000000000 ) ) ;
#3121 = APPLICATION_CONTEXT ( 'automotive_design' ) ;
#3122 = ORIENTED_EDGE ( 'NONE', *, *, #14648, .T. ) ;
#3123 = CARTESIAN_POINT ( 'NONE',  ( 1.749999999999998002, 24.89775460606851354, -12.96210679857759729 ) ) ;
#3124 = DIRECTION ( 'NONE',  ( 0.1643989873053578465, -0.9863939238321436376, 0.000000000000000000 ) ) ;
#3125 = VECTOR ( 'NONE', #6109, 1000.000000000000227 ) ;
#3126 = ORIENTED_EDGE ( 'NONE', *, *, #5165, .F. ) ;
#3127 = AXIS2_PLACEMENT_3D ( 'NONE', #8280, #9361, #14279 ) ;
#3128 = CARTESIAN_POINT ( 'NONE',  ( 0.5431871198829544278, 3.619024283482072946, 16.57708379306446034 ) ) ;
#3129 = EDGE_LOOP ( 'NONE', ( #8096, #6258, #6785, #2613, #8197, #2655 ) ) ;
#3130 = CIRCLE ( 'NONE', #9752, 2.524999999999996803 ) ;
#3131 = EDGE_LOOP ( 'NONE', ( #11039, #2236, #4649, #15148 ) ) ;
#3132 = CARTESIAN_POINT ( 'NONE',  ( 0.02531912748464848137, 2.311161484776556030, 14.46287784598618309 ) ) ;
#3133 = EDGE_CURVE ( 'NONE', #7072, #9975, #11387, .T. ) ;
#3134 = DIRECTION ( 'NONE',  ( 0.000000000000000000, 0.000000000000000000, 1.000000000000000000 ) ) ;
#3135 = EDGE_CURVE ( 'NONE', #13302, #7167, #4785, .T. ) ;
#3136 = CIRCLE ( 'NONE', #2885, 28.06981291497571362 ) ;
#3137 = CARTESIAN_POINT ( 'NONE',  ( 2.789999999999999147, 9.324097380959765147, -22.25075486061728824 ) ) ;
#3138 = CARTESIAN_POINT ( 'NONE',  ( 0.07181525696555295102, -5.344212458769539431, 24.78695292654919768 ) ) ;
#3139 = CARTESIAN_POINT ( 'NONE',  ( 1.749999999999999778, 17.29145405592695539, -4.835383649608290924 ) ) ;
#3140 = CARTESIAN_POINT ( 'NONE',  ( 2.764680872515351329, 14.46287784598617421, -2.311161484776606212 ) ) ;
#3141 = DIRECTION ( 'NONE',  ( 0.000000000000000000, 0.000000000000000000, 1.000000000000000000 ) ) ;
#3142 = VERTEX_POINT ( 'NONE', #6918 ) ;
#3143 = DIRECTION ( 'NONE',  ( -0.4571871344001417481, -0.8893705212896291235, 0.000000000000000000 ) ) ;
#3144 = CARTESIAN_POINT ( 'NONE',  ( -0.1717365941144614327, -6.008326913195983998, -0.8000000000000000444 ) ) ;
#3145 = CARTESIAN_POINT ( 'NONE',  ( 2.764680872515351329, -11.36963888406680923, -9.232963481057881339 ) ) ;
#3146 = EDGE_LOOP ( 'NONE', ( #2363, #4011, #8226, #1875, #3971, #5105, #9866 ) ) ;
#3147 = CIRCLE ( 'NONE', #12705, 4.000000000000000888 ) ;
#3148 = EDGE_CURVE ( 'NONE', #15013, #10097, #6002, .T. ) ;
#3149 = CARTESIAN_POINT ( 'NONE',  ( 2.790000000000000924, 0.000000000000000000, 0.000000000000000000 ) ) ;
#3151 = AXIS2_PLACEMENT_3D ( 'NONE', #6810, #1899, #5594 ) ;
#3150 = CARTESIAN_POINT ( 'NONE',  ( 3.751931928061364552, -0.6025004624012525456, 6.999999999999989342 ) ) ;
#3152 = VERTEX_POINT ( 'NONE', #11523 ) ;
#3153 = CIRCLE ( 'NONE', #11234, 0.1000000000000002554 ) ;
#3154 = VERTEX_POINT ( 'NONE', #13830 ) ;
#3155 = CARTESIAN_POINT ( 'NONE',  ( 2.031033491000350466, -24.80232951178386713, 12.05173163741713083 ) ) ;
#3156 = CARTESIAN_POINT ( 'NONE',  ( -14.40394475573011945, -4.794738323547946379, 22.00000000000000000 ) ) ;
#3157 = EDGE_LOOP ( 'NONE', ( #2550, #11441 ) ) ;
#3158 = CYLINDRICAL_SURFACE ( 'NONE', #6590, 9.999999999999994671 ) ;
#3159 = LINE ( 'NONE', #3298, #8682 ) ;
#3160 = CARTESIAN_POINT ( 'NONE',  ( 2.765633920072235963, -5.391175441198450713, -24.15498966839968276 ) ) ;
#3161 = CIRCLE ( 'NONE', #2413, 24.12539914357697413 ) ;
#3162 = CARTESIAN_POINT ( 'NONE',  ( 0.1882238552569851786, -23.64332819722389090, 10.68696068830398360 ) ) ;
#3163 = CARTESIAN_POINT ( 'NONE',  ( 5.999999999999999112, 7.347880794884118750E-16, 3.895000000000000462 ) ) ;
#3164 = ORIENTED_EDGE ( 'NONE', *, *, #9841, .T. ) ;
#3165 = FACE_OUTER_BOUND ( 'NONE', #12101, .T. ) ;
#3166 = AXIS2_PLACEMENT_3D ( 'NONE', #8480, #5049, #14647 ) ;
#3167 = CIRCLE ( 'NONE', #1441, 4.000000000000000888 ) ;
#3168 = DIRECTION ( 'NONE',  ( -0.9148936170212765839, -0.4036950204470271530, 0.000000000000000000 ) ) ;
#3169 = ORIENTED_EDGE ( 'NONE', *, *, #12361, .T. ) ;
#3170 = CARTESIAN_POINT ( 'NONE',  ( 0.000000000000000000, 0.000000000000000000, -10.00000000000000888 ) ) ;
#3171 = ORIENTED_EDGE ( 'NONE', *, *, #8319, .F. ) ;
#3172 = VERTEX_POINT ( 'NONE', #7995 ) ;
#3173 = ORIENTED_EDGE ( 'NONE', *, *, #2929, .T. ) ;
#3174 = CARTESIAN_POINT ( 'NONE',  ( 2.764680872513205934, -11.36963888406694068, 9.232963481057725019 ) ) ;
#3175 = EDGE_CURVE ( 'NONE', #8536, #13456, #11595, .T. ) ;
#3176 = CIRCLE ( 'NONE', #2675, 2.524999999999996803 ) ;
#3177 = CIRCLE ( 'NONE', #8312, 17.95481323787947758 ) ;
#3178 = CIRCLE ( 'NONE', #7357, 2.524999999999999023 ) ;
#3179 = CARTESIAN_POINT ( 'NONE',  ( 1.749999999999998002, -12.96210679857804671, 24.89775460606827551 ) ) ;
#3180 = ORIENTED_EDGE ( 'NONE', *, *, #6159, .F. ) ;
#3181 = FACE_OUTER_BOUND ( 'NONE', #5045, .T. ) ;
#3182 = DIRECTION ( 'NONE',  ( 1.000000000000000000, 0.000000000000000000, 0.000000000000000000 ) ) ;
#3183 = PRODUCT_DEFINITION ( 'UNKNOWN', '', #12605, #6399 ) ;
#3184 = ADVANCED_FACE ( 'NONE', ( #2160 ), #6846, .T. ) ;
#3185 = DIRECTION ( 'NONE',  ( 0.000000000000000000, 0.000000000000000000, -1.000000000000000000 ) ) ;
#3186 = EDGE_CURVE ( 'NONE', #1061, #9201, #4543, .T. ) ;
#3187 = AXIS2_PLACEMENT_3D ( 'NONE', #2541, #8225, #3616 ) ;
#3188 = CARTESIAN_POINT ( 'NONE',  ( 0.7592463941534238758, 3.797885586973211325, 27.31305418910211458 ) ) ;
#3189 = ORIENTED_EDGE ( 'NONE', *, *, #5076, .F. ) ;
#3190 = CARTESIAN_POINT ( 'NONE',  ( 0.02436607992776194942, -5.391175441198450713, -24.15498966839968276 ) ) ;
#3191 = DIRECTION ( 'NONE',  ( -1.000000000000000000, -0.000000000000000000, -0.000000000000000000 ) ) ;
#3192 = ORIENTED_EDGE ( 'NONE', *, *, #10838, .T. ) ;
#3193 = ORIENTED_EDGE ( 'NONE', *, *, #7385, .F. ) ;
#3194 = DIRECTION ( 'NONE',  ( 0.000000000000000000, 0.000000000000000000, 1.000000000000000000 ) ) ;
#3195 = EDGE_CURVE ( 'NONE', #12453, #8792, #5770, .T. ) ;
#3196 = AXIS2_PLACEMENT_3D ( 'NONE', #13510, #7965, #11195 ) ;
#3197 = EDGE_CURVE ( 'NONE', #13784, #6657, #10149, .T. ) ;
#3198 = VERTEX_POINT ( 'NONE', #11372 ) ;
#3199 = CARTESIAN_POINT ( 'NONE',  ( 2.790000000000060876, -8.842064619038600526, 11.12234047011187421 ) ) ;
#3201 = ORIENTED_EDGE ( 'NONE', *, *, #14543, .F. ) ;
#3200 = EDGE_CURVE ( 'NONE', #11548, #15218, #8496, .T. ) ;
#3202 = CARTESIAN_POINT ( 'NONE',  ( -14.40394475573011945, -10.79473832354794460, -3.799999999999999822 ) ) ;
#3203 = CARTESIAN_POINT ( 'NONE',  ( 2.789999999999999147, -24.15498966839966855, 5.391175441198523544 ) ) ;
#3204 = ORIENTED_EDGE ( 'NONE', *, *, #7686, .F. ) ;
#3205 = CARTESIAN_POINT ( 'NONE',  ( 2.718184745196085661, 12.74223776959200727, 21.92234060054350309 ) ) ;
#3206 = CARTESIAN_POINT ( 'NONE',  ( 1.149999999999998135, 0.000000000000000000, -4.000000000000000000 ) ) ;
#3207 = VERTEX_POINT ( 'NONE', #10225 ) ;
#3208 = AXIS2_PLACEMENT_3D ( 'NONE', #9497, #10509, #14191 ) ;
#3209 = EDGE_CURVE ( 'NONE', #4384, #13626, #1230, .T. ) ;
#3210 = EDGE_LOOP ( 'NONE', ( #8081, #14742, #11925, #14374, #11488 ) ) ;
#3211 = CARTESIAN_POINT ( 'NONE',  ( -18.40394475573011945, -10.79473832354794460, 12.00000000000000000 ) ) ;
#3212 = DIRECTION ( 'NONE',  ( 0.000000000000000000, 0.000000000000000000, 1.000000000000000000 ) ) ;
#3213 = CARTESIAN_POINT ( 'NONE',  ( -14.40394475573012301, -16.79473832354794993, 16.99999999999999645 ) ) ;
#3214 = LINE ( 'NONE', #9275, #1336 ) ;
#3215 = CARTESIAN_POINT ( 'NONE',  ( 88.46153288930041469, 16.46030115554384565, 6.000000000000000000 ) ) ;
#3216 = CARTESIAN_POINT ( 'NONE',  ( 0.000000000000000000, 0.000000000000000000, -0.8000000000000000444 ) ) ;
#3217 = B_SPLINE_CURVE_WITH_KNOTS ( 'NONE', 3,
 ( #12126, #1838, #8604, #10986 ),
 .UNSPECIFIED., .F., .F.,
 ( 4, 4 ),
 ( 0.005258120783916782857, 0.005948386350302925507 ),
 .UNSPECIFIED. ) ;
#3218 = ORIENTED_EDGE ( 'NONE', *, *, #8150, .F. ) ;
#3219 = DIRECTION ( 'NONE',  ( -1.000000000000000000, 0.000000000000000000, 0.000000000000000000 ) ) ;
#3220 = CARTESIAN_POINT ( 'NONE',  ( 0.000000000000000000, 0.000000000000000000, 3.895000000000000462 ) ) ;
#3221 = CARTESIAN_POINT ( 'NONE',  ( 74.00000000000000000, 7.347880794884117764E-16, 4.500000000000000888 ) ) ;
#3222 = ORIENTED_EDGE ( 'NONE', *, *, #10042, .T. ) ;
#3223 = FACE_OUTER_BOUND ( 'NONE', #6680, .T. ) ;
#3224 = FACE_BOUND ( 'NONE', #14200, .T. ) ;
#3225 = ORIENTED_EDGE ( 'NONE', *, *, #5906, .F. ) ;
#3226 = ORIENTED_EDGE ( 'NONE', *, *, #11081, .T. ) ;
#3227 = CARTESIAN_POINT ( 'NONE',  ( 2.718131914667132776, -23.19485392143220182, 10.24630254990507083 ) ) ;
#3228 = CYLINDRICAL_SURFACE ( 'NONE', #11719, 17.95481323787947403 ) ;
#3229 = ORIENTED_EDGE ( 'NONE', *, *, #12328, .F. ) ;
#3230 = CARTESIAN_POINT ( 'NONE',  ( 2.789999999999999147, 1.948757464274366136, -13.87420763704359139 ) ) ;
#3231 = CARTESIAN_POINT ( 'NONE',  ( 0.02436607992776194942, -5.391175441198450713, -24.15498966839968276 ) ) ;
#3232 = DIRECTION ( 'NONE',  ( 0.000000000000000000, 0.000000000000000000, 1.000000000000000000 ) ) ;
#3233 = CARTESIAN_POINT ( 'NONE',  ( 0.1882238552569850676, 23.64332819722396195, -10.68696068830383084 ) ) ;
#3234 = CARTESIAN_POINT ( 'NONE',  ( 2.071132347512118166, 24.19190980169967631, 12.96989951879416658 ) ) ;
#3235 = VERTEX_POINT ( 'NONE', #7146 ) ;
#3236 = B_SPLINE_CURVE_WITH_KNOTS ( 'NONE', 3,
 ( #9166, #6936, #2177, #13847, #8094, #15089, #4563, #9244 ),
 .UNSPECIFIED., .F., .F.,
 ( 4, 2, 2, 4 ),
 ( 4.663089413031289195E-07, 0.001898630173449298219, 0.002847712105703296016, 0.003796794037957293595 ),
 .UNSPECIFIED. ) ;
#3237 = DIRECTION ( 'NONE',  ( 0.000000000000000000, 0.000000000000000000, 1.000000000000000000 ) ) ;
#3238 = CARTESIAN_POINT ( 'NONE',  ( 0.000000000000000000, 4.898587196589412829E-16, -4.000000000000000000 ) ) ;
#3239 = EDGE_LOOP ( 'NONE', ( #14240, #4911 ) ) ;
#3240 = B_SPLINE_CURVE_WITH_KNOTS ( 'NONE', 3,
 ( #13429, #6363, #1600, #14521, #9662, #14361 ),
 .UNSPECIFIED., .F., .F.,
 ( 4, 2, 4 ),
 ( 2.321268216997177022E-07, 0.001878622960950496190, 0.003757013795079292354 ),
 .UNSPECIFIED. ) ;
#3241 = ORIENTED_EDGE ( 'NONE', *, *, #8434, .F. ) ;
#3242 = VERTEX_POINT ( 'NONE', #2463 ) ;
#3243 = ORIENTED_EDGE ( 'NONE', *, *, #7762, .F. ) ;
#3244 = CARTESIAN_POINT ( 'NONE',  ( 1.250000000000001110, 0.000000000000000000, 0.000000000000000000 ) ) ;
#3245 = CARTESIAN_POINT ( 'NONE',  ( 0.02436607992776758727, 24.15498966839963302, 5.391175441198700291 ) ) ;
#3246 = CARTESIAN_POINT ( 'NONE',  ( 2.740003281797977586, -5.264737421541426876, -13.99876742897264847 ) ) ;
#3247 = DIRECTION ( 'NONE',  ( -1.000000000000000000, -0.000000000000000000, 0.000000000000000000 ) ) ;
#3248 = EDGE_CURVE ( 'NONE', #546, #10097, #10419, .T. ) ;
#3249 = ORIENTED_EDGE ( 'NONE', *, *, #10369, .F. ) ;
#3250 = DIRECTION ( 'NONE',  ( -1.000000000000000000, -0.000000000000000000, -0.000000000000000000 ) ) ;
#3251 = CARTESIAN_POINT ( 'NONE',  ( -1.000000000000000222, -4.808326913195983821, -0.8000000000000000444 ) ) ;
#3252 = ADVANCED_FACE ( 'NONE', ( #6143 ), #11667, .F. ) ;
#3253 = CARTESIAN_POINT ( 'NONE',  ( 0.7188676524878460095, -24.19190980169966210, 12.96989951879399428 ) ) ;
#3254 = EDGE_LOOP ( 'NONE', ( #9313, #14348, #6943, #14316 ) ) ;
#3255 = DIRECTION ( 'NONE',  ( -1.000000000000000000, 0.000000000000000000, 0.000000000000000000 ) ) ;
#3256 = CARTESIAN_POINT ( 'NONE',  ( 69.97572749000833880, 15.55805301486455683, 7.000000000000000000 ) ) ;
#3257 = ORIENTED_EDGE ( 'NONE', *, *, #13814, .T. ) ;
#3258 = ORIENTED_EDGE ( 'NONE', *, *, #1540, .T. ) ;
#3259 = EDGE_CURVE ( 'NONE', #12986, #1724, #4294, .T. ) ;
#3260 = VECTOR ( 'NONE', #11218, 1000.000000000000000 ) ;
#3261 = EDGE_CURVE ( 'NONE', #1993, #8917, #12384, .T. ) ;
#3262 = ORIENTED_EDGE ( 'NONE', *, *, #8026, .T. ) ;
#3263 = FACE_OUTER_BOUND ( 'NONE', #7626, .T. ) ;
#3264 = CARTESIAN_POINT ( 'NONE',  ( -14.40394475573012301, -4.794738323547945491, 19.99999999999999645 ) ) ;
#3265 = DIRECTION ( 'NONE',  ( 1.000000000000000000, 0.000000000000000000, 0.000000000000000000 ) ) ;
#3266 = MANIFOLD_SOLID_BREP ( 'OuterRace', #9908 ) ;
#3267 = ORIENTED_EDGE ( 'NONE', *, *, #8626, .F. ) ;
#3268 = CARTESIAN_POINT ( 'NONE',  ( 70.16198417812034904, 9.730076655429538590, 2.999999999999999112 ) ) ;
#3269 = ORIENTED_EDGE ( 'NONE', *, *, #8754, .F. ) ;
#3270 = ADVANCED_FACE ( 'NONE', ( #210 ), #8291, .T. ) ;
#3271 = VERTEX_POINT ( 'NONE', #10537 ) ;
#3272 = CARTESIAN_POINT ( 'NONE',  ( 61.98919079003883326, 3.953582723775848962, 7.000000000000000000 ) ) ;
#3273 = DIRECTION ( 'NONE',  ( 0.4036950204470283188, -0.9148936170212761398, -0.000000000000000000 ) ) ;
#3274 = EDGE_CURVE ( 'NONE', #797, #6094, #4929, .T. ) ;
#3275 = ADVANCED_FACE ( 'NONE', ( #1456 ), #9668, .T. ) ;
#3276 = DIRECTION ( 'NONE',  ( 0.000000000000000000, 0.000000000000000000, 1.000000000000000000 ) ) ;
#3277 = DIRECTION ( 'NONE',  ( -0.9995917534020515305, -0.02857142857142857054, 0.000000000000000000 ) ) ;
#3278 = CONTEXT_DEPENDENT_SHAPE_REPRESENTATION ( #10473, #15002 ) ;
#3279 = DIRECTION ( 'NONE',  ( 0.000000000000000000, 0.000000000000000000, -1.000000000000000000 ) ) ;
#3280 = CARTESIAN_POINT ( 'NONE',  ( 2.790000000000000036, -15.96500990068111214, -18.34424029220128816 ) ) ;
#3281 = EDGE_CURVE ( 'NONE', #8350, #929, #1537, .T. ) ;
#3282 = ORIENTED_EDGE ( 'NONE', *, *, #12297, .F. ) ;
#3283 = LINE ( 'NONE', #10126, #11495 ) ;
#3284 = CARTESIAN_POINT ( 'NONE',  ( 0.000000000000000000, -9.324097380959319281, -22.25075486061748009 ) ) ;
#3285 = LINE ( 'NONE', #6675, #1640 ) ;
#3286 = ORIENTED_EDGE ( 'NONE', *, *, #11552, .F. ) ;
#3287 = VERTEX_POINT ( 'NONE', #9370 ) ;
#3288 = CARTESIAN_POINT ( 'NONE',  ( 2.789999999999999147, -9.836394144775869819, 22.71065055754449347 ) ) ;
#3289 = CARTESIAN_POINT ( 'NONE',  ( 2.262072625383134472, 4.996265754456739927, -26.57710921259756631 ) ) ;
#3290 = ORIENTED_EDGE ( 'NONE', *, *, #7125, .F. ) ;
#3291 = AXIS2_PLACEMENT_3D ( 'NONE', #6878, #11558, #15191 ) ;
#3292 = VERTEX_POINT ( 'NONE', #12818 ) ;
#3293 = FACE_OUTER_BOUND ( 'NONE', #3911, .T. ) ;
#3294 = CARTESIAN_POINT ( 'NONE',  ( 80.00000000000000000, 0.000000000000000000, 4.500000000000003553 ) ) ;
#3295 = ORIENTED_EDGE ( 'NONE', *, *, #8552, .T. ) ;
#3296 = CIRCLE ( 'NONE', #9414, 24.12539914357697413 ) ;
#3297 = CARTESIAN_POINT ( 'NONE',  ( 2.765633920072239516, 16.37294372382858398, 18.55949924794898465 ) ) ;
#3298 = CARTESIAN_POINT ( 'NONE',  ( 1.394999999999999574, 17.39253030560841751, 4.458161950358562109 ) ) ;
#3299 = DIRECTION ( 'NONE',  ( -0.9914448613738103822, -0.1305261922200521840, 0.000000000000000000 ) ) ;
#3300 = CARTESIAN_POINT ( 'NONE',  ( 66.02295749185037721, 31.67615731643408949, 4.000000000000000000 ) ) ;
#3301 = CARTESIAN_POINT ( 'NONE',  ( 2.765633920072239516, 21.30679549418631780, 12.59161484032919986 ) ) ;
#3302 = EDGE_CURVE ( 'NONE', #3709, #8012, #6990, .T. ) ;
#3303 = VERTEX_POINT ( 'NONE', #12044 ) ;
#3304 = CARTESIAN_POINT ( 'NONE',  ( 2.789999999999999147, -7.739906618939614624, -10.88091150984234545 ) ) ;
#3305 = AXIS2_PLACEMENT_3D ( 'NONE', #3104, #1792, #11316 ) ;
#3306 = LINE ( 'NONE', #6768, #5754 ) ;
#3307 = ORIENTED_EDGE ( 'NONE', *, *, #9380, .T. ) ;
#3308 = VERTEX_POINT ( 'NONE', #1685 ) ;
#3309 = ORIENTED_EDGE ( 'NONE', *, *, #8893, .F. ) ;
#3310 = EDGE_LOOP ( 'NONE', ( #3692, #3204, #9881, #5251, #9880, #10633, #6463 ) ) ;
#3311 = DIRECTION ( 'NONE',  ( 1.000000000000000000, 0.000000000000000000, 0.000000000000000000 ) ) ;
#3312 = TOROIDAL_SURFACE ( 'NONE', #7236, 24.12539914357697768, 8.000000000000000000 ) ;
#3313 = CIRCLE ( 'NONE', #12392, 4.000000000000000000 ) ;
#3314 = CIRCLE ( 'NONE', #11891, 24.12539914357697413 ) ;
#3315 = DIRECTION ( 'NONE',  ( -1.000000000000000000, -0.000000000000000000, -0.000000000000000000 ) ) ;
#3316 =( REPRESENTATION_RELATIONSHIP ('NONE','NONE', #12685, #13067 ) REPRESENTATION_RELATIONSHIP_WITH_TRANSFORMATION ( #2123 )SHAPE_REPRESENTATION_RELATIONSHIP( ) );
#3317 = EDGE_CURVE ( 'NONE', #367, #12499, #9243, .T. ) ;
#3318 = CARTESIAN_POINT ( 'NONE',  ( -14.40394475573011235, 8.328953704812679362E-15, 16.99999999999999645 ) ) ;
#3319 = ORIENTED_EDGE ( 'NONE', *, *, #8722, .T. ) ;
#3320 = CARTESIAN_POINT ( 'NONE',  ( 88.46153288930041469, 16.46030115554384565, 2.999999999999999112 ) ) ;
#3321 = CARTESIAN_POINT ( 'NONE',  ( 0.02436607992776368414, 18.55949924794916228, -16.37294372382838148 ) ) ;
#3322 = AXIS2_PLACEMENT_3D ( 'NONE', #14871, #4342, #3194 ) ;
#3323 = CIRCLE ( 'NONE', #7734, 2.524999999999995914 ) ;
#3324 = CARTESIAN_POINT ( 'NONE',  ( 2.765633920072239516, 21.30679549418631780, 12.59161484032919986 ) ) ;
#3325 = EDGE_CURVE ( 'NONE', #9731, #15027, #14526, .T. ) ;
#3326 = ORIENTED_EDGE ( 'NONE', *, *, #11310, .T. ) ;
#3327 = DIRECTION ( 'NONE',  ( -1.000000000000000000, -0.000000000000000000, -0.000000000000000000 ) ) ;
#3328 = PRODUCT_DEFINITION_SHAPE ( 'NONE', 'NONE',  #15242 ) ;
#3329 = EDGE_CURVE ( 'NONE', #9761, #6202, #5388, .T. ) ;
#3330 = DIRECTION ( 'NONE',  ( 0.000000000000000000, 0.000000000000000000, 1.000000000000000000 ) ) ;
#3331 = ORIENTED_EDGE ( 'NONE', *, *, #4868, .F. ) ;
#3332 = ORIENTED_EDGE ( 'NONE', *, *, #5735, .F. ) ;
#3333 = AXIS2_PLACEMENT_3D ( 'NONE', #538, #2855, #10920 ) ;
#3334 = FACE_OUTER_BOUND ( 'NONE', #753, .T. ) ;
#3335 = ORIENTED_EDGE ( 'NONE', *, *, #1686, .F. ) ;
#3336 = CARTESIAN_POINT ( 'NONE',  ( -14.40394475573011945, -10.79473832354794283, -3.000000000000000000 ) ) ;
#3337 = CARTESIAN_POINT ( 'NONE',  ( 2.783025342027734883, 23.92335783895644852, -5.408388659523843067 ) ) ;
#3338 = CARTESIAN_POINT ( 'NONE',  ( 2.550660015654387269, -15.07093484180036924, 5.269646308239033239 ) ) ;
#3339 = B_SPLINE_CURVE_WITH_KNOTS ( 'NONE', 3,
 ( #10741, #14044, #2291, #198 ),
 .UNSPECIFIED., .F., .F.,
 ( 4, 4 ),
 ( 2.135345996700793610E-07, 0.0006888010880211471818 ),
 .UNSPECIFIED. ) ;
#3340 = ORIENTED_EDGE ( 'NONE', *, *, #297, .F. ) ;
#3341 = AXIS2_PLACEMENT_3D ( 'NONE', #9065, #5610, #8898 ) ;
#3342 = FILL_AREA_STYLE_COLOUR ( '', #11696 ) ;
#3343 = EDGE_CURVE ( 'NONE', #12627, #6646, #13899, .T. ) ;
#3344 = CARTESIAN_POINT ( 'NONE',  ( 3.799999999999999378, 0.000000000000000000, -0.8000000000000000444 ) ) ;
#3345 = VERTEX_POINT ( 'NONE', #4150 ) ;
#3346 = VERTEX_POINT ( 'NONE', #7605 ) ;
#3347 = CARTESIAN_POINT ( 'NONE',  ( 0.7795480763126747537, -12.70439593876652218, -11.98750039041507343 ) ) ;
#3348 = CARTESIAN_POINT ( 'NONE',  ( 2.789999999999999147, -7.334849878007332791, -23.31896751603339979 ) ) ;
#3349 = AXIS2_PLACEMENT_3D ( 'NONE', #12201, #6369, #2912 ) ;
#3350 = EDGE_CURVE ( 'NONE', #9228, #555, #15090, .T. ) ;
#3351 = DIRECTION ( 'NONE',  ( -0.000000000000000000, -0.000000000000000000, 1.000000000000000000 ) ) ;
#3352 = DIRECTION ( 'NONE',  ( -0.4036950204470285408, 0.9148936170212760288, 0.000000000000000000 ) ) ;
#3353 = CONTEXT_DEPENDENT_SHAPE_REPRESENTATION ( #954, #4566 ) ;
#3354 = CARTESIAN_POINT ( 'NONE',  ( 75.68384697807671557, 11.35494834827056110, 2.999999999999999112 ) ) ;
#3355 = AXIS2_PLACEMENT_3D ( 'NONE', #5126, #7491, #14495 ) ;
#3356 =( GEOMETRIC_REPRESENTATION_CONTEXT ( 3 ) GLOBAL_UNCERTAINTY_ASSIGNED_CONTEXT ( ( #6240 ) ) GLOBAL_UNIT_ASSIGNED_CONTEXT ( ( #13124, #12892, #2382 ) ) REPRESENTATION_CONTEXT ( 'NONE', 'WORKASPACE' ) );
#3357 = CARTESIAN_POINT ( 'NONE',  ( 2.604434325169353137, -25.77772010606608077, 2.851997810081559503 ) ) ;
#3358 = VECTOR ( 'NONE', #1037, 1000.000000000000000 ) ;
#3359 = VERTEX_POINT ( 'NONE', #10974 ) ;
#3360 = FACE_OUTER_BOUND ( 'NONE', #14931, .T. ) ;
#3361 = CARTESIAN_POINT ( 'NONE',  ( -0.4472135954999577612, 0.000000000000000000, -4.599999999999999645 ) ) ;
#3362 = CARTESIAN_POINT ( 'NONE',  ( 0.7592463896980037319, 19.12676442129342647, 19.86438386685667368 ) ) ;
#3363 = FACE_OUTER_BOUND ( 'NONE', #11153, .T. ) ;
#3364 = EDGE_CURVE ( 'NONE', #8684, #5234, #9894, .T. ) ;
#3365 = EDGE_CURVE ( 'NONE', #2017, #7876, #9196, .T. ) ;
#3366 = VECTOR ( 'NONE', #10430, 1000.000000000000000 ) ;
#3367 = ORIENTED_EDGE ( 'NONE', *, *, #1269, .F. ) ;
#3368 = CARTESIAN_POINT ( 'NONE',  ( 58.14665764790533586, -0.9105996816177489572, 7.000000000000000000 ) ) ;
#3369 = CARTESIAN_POINT ( 'NONE',  ( 0.02436607992775544421, -22.71065055754445439, -9.836394144775947979 ) ) ;
#3370 = ORIENTED_EDGE ( 'NONE', *, *, #8629, .T. ) ;
#3371 = CIRCLE ( 'NONE', #11691, 3.000000000000002665 ) ;
#3372 = EDGE_LOOP ( 'NONE', ( #4026, #6931, #12680, #15039 ) ) ;
#3373 = VECTOR ( 'NONE', #12808, 1000.000000000000000 ) ;
#3374 = DIRECTION ( 'NONE',  ( -1.000000000000000000, -0.000000000000000000, -0.000000000000000000 ) ) ;
#3375 = DIRECTION ( 'NONE',  ( -0.000000000000000000, -0.000000000000000000, -1.000000000000000000 ) ) ;
#3376 = VERTEX_POINT ( 'NONE', #11054 ) ;
#3377 = AXIS2_PLACEMENT_3D ( 'NONE', #9765, #2767, #5398 ) ;
#3378 = CARTESIAN_POINT ( 'NONE',  ( 0.000000000000000000, 0.4273491293402468805, -0.8000000000000000444 ) ) ;
#3379 = CARTESIAN_POINT ( 'NONE',  ( -9.403944755730117677, -7.794738323547949044, 16.99999999999999645 ) ) ;
#3380 = DIRECTION ( 'NONE',  ( -1.000000000000000000, -0.000000000000000000, 0.000000000000000000 ) ) ;
#3381 = FACE_OUTER_BOUND ( 'NONE', #8542, .T. ) ;
#3382 = EDGE_CURVE ( 'NONE', #5968, #13607, #6738, .T. ) ;
#3383 = ADVANCED_FACE ( 'NONE', ( #7672 ), #10180, .T. ) ;
#3384 = EDGE_LOOP ( 'NONE', ( #13328, #11974, #808, #11831, #14932, #8297 ) ) ;
#3385 = CARTESIAN_POINT ( 'NONE',  ( 8.000000000000000000, 0.000000000000000000, 0.000000000000000000 ) ) ;
#3386 = VECTOR ( 'NONE', #10740, 1000.000000000000000 ) ;
#3387 = CARTESIAN_POINT ( 'NONE',  ( -14.40394475573012301, -7.794738323547949932, 16.99999999999999645 ) ) ;
#3388 = ADVANCED_FACE ( 'NONE', ( #8739 ), #4542, .T. ) ;
#3389 = AXIS2_PLACEMENT_3D ( 'NONE', #4691, #10814, #4989 ) ;
#3390 = VERTEX_POINT ( 'NONE', #440 ) ;
#3391 = CIRCLE ( 'NONE', #10264, 2.524999999999995914 ) ;
#3392 = VERTEX_POINT ( 'NONE', #13516 ) ;
#3393 = EDGE_LOOP ( 'NONE', ( #12793, #3112, #5373, #10201 ) ) ;
#3394 = VERTEX_POINT ( 'NONE', #2914 ) ;
#3395 = FACE_OUTER_BOUND ( 'NONE', #2081, .T. ) ;
#3396 = ADVANCED_FACE ( 'NONE', ( #12352 ), #397, .T. ) ;
#3397 = B_SPLINE_CURVE_WITH_KNOTS ( 'NONE', 3,
 ( #5910, #39, #322, #4752, #9422, #2446 ),
 .UNSPECIFIED., .F., .F.,
 ( 4, 2, 4 ),
 ( 2.132675795046084789E-07, 0.001878604073277003903, 0.003756994878974503470 ),
 .UNSPECIFIED. ) ;
#3398 = AXIS2_PLACEMENT_3D ( 'NONE', #6412, #325, #13321 ) ;
#3399 = DIRECTION ( 'NONE',  ( 1.000000000000000000, 0.000000000000000000, 0.000000000000000000 ) ) ;
#3400 = DIRECTION ( 'NONE',  ( 1.000000000000000000, 0.000000000000000000, 0.000000000000000000 ) ) ;
#3401 = LINE ( 'NONE', #1947, #4671 ) ;
#3402 = B_SPLINE_CURVE_WITH_KNOTS ( 'NONE', 3,
 ( #3802, #4903, #9495, #14336 ),
 .UNSPECIFIED., .F., .F.,
 ( 4, 4 ),
 ( 0.005123713096549377226, 0.005814346476695809313 ),
 .UNSPECIFIED. ) ;
#3403 = VERTEX_POINT ( 'NONE', #2691 ) ;
#3404 = CARTESIAN_POINT ( 'NONE',  ( 1.250000000000001110, 7.286648454926751965E-16, 5.899999999999999467 ) ) ;
#3405 = CARTESIAN_POINT ( 'NONE',  ( 2.789999999999999147, 0.000000000000000000, 0.000000000000000000 ) ) ;
#3406 = MECHANICAL_DESIGN_GEOMETRIC_PRESENTATION_REPRESENTATION (  '', ( #1170 ), #10495 ) ;
#3407 = EDGE_LOOP ( 'NONE', ( #12891, #871, #12534, #2968, #14703, #11524 ) ) ;
#3408 = FACE_OUTER_BOUND ( 'NONE', #9800, .T. ) ;
#3409 = DIRECTION ( 'NONE',  ( 0.000000000000000000, 0.000000000000000000, 1.000000000000000000 ) ) ;
#3410 = VERTEX_POINT ( 'NONE', #2832 ) ;
#3411 = ORIENTED_EDGE ( 'NONE', *, *, #5994, .F. ) ;
#3412 = EDGE_CURVE ( 'NONE', #269, #13647, #6561, .T. ) ;
#3413 = CARTESIAN_POINT ( 'NONE',  ( 80.00000000000000000, 0.000000000000000000, -130.1575142076926852 ) ) ;
#3414 = EDGE_LOOP ( 'NONE', ( #4812, #2695, #15056, #9225 ) ) ;
#3415 = CYLINDRICAL_SURFACE ( 'NONE', #1088, 13.19999999999999929 ) ;
#3416 = CARTESIAN_POINT ( 'NONE',  ( 1.749999999999998002, 0.000000000000000000, 0.000000000000000000 ) ) ;
#3417 = EDGE_CURVE ( 'NONE', #9424, #14731, #8596, .T. ) ;
#3418 = DIRECTION ( 'NONE',  ( 0.000000000000000000, 0.000000000000000000, 1.000000000000000000 ) ) ;
#3419 = DIRECTION ( 'NONE',  ( -1.000000000000000000, -0.000000000000000000, 0.000000000000000000 ) ) ;
#3420 = ORIENTED_EDGE ( 'NONE', *, *, #10811, .F. ) ;
#3421 = CARTESIAN_POINT ( 'NONE',  ( 0.000000000000000000, 0.000000000000000000, 10.00000000000000000 ) ) ;
#3422 = LINE ( 'NONE', #10635, #3358 ) ;
#3423 = ORIENTED_EDGE ( 'NONE', *, *, #11, .F. ) ;
#3424 = ORIENTED_EDGE ( 'NONE', *, *, #817, .T. ) ;
#3425 = CARTESIAN_POINT ( 'NONE',  ( 66.02295749185039142, 31.67615731643408949, 2.000000000000000000 ) ) ;
#3426 = CIRCLE ( 'NONE', #4417, 6.000000000000005329 ) ;
#3427 = CARTESIAN_POINT ( 'NONE',  ( 2.765633920072235963, 21.30679549418649543, -12.59161484032888723 ) ) ;
#3428 = CARTESIAN_POINT ( 'NONE',  ( -10.00000000000000000, 0.000000000000000000, 0.000000000000000000 ) ) ;
#3429 = CYLINDRICAL_SURFACE ( 'NONE', #5543, 2.524999999999995914 ) ;
#3430 = DIRECTION ( 'NONE',  ( -1.000000000000000000, 0.000000000000000000, 0.000000000000000000 ) ) ;
#3431 = DIRECTION ( 'NONE',  ( 0.000000000000000000, 0.000000000000000000, 1.000000000000000000 ) ) ;
#3432 = EDGE_CURVE ( 'NONE', #9629, #10133, #2715, .T. ) ;
#3433 = ORIENTED_EDGE ( 'NONE', *, *, #5924, .T. ) ;
#3434 = DIRECTION ( 'NONE',  ( 0.000000000000000000, 0.000000000000000000, 1.000000000000000000 ) ) ;
#3435 = DIRECTION ( 'NONE',  ( -1.000000000000000000, 0.000000000000000000, 0.000000000000000000 ) ) ;
#3436 = LINE ( 'NONE', #1208, #3855 ) ;
#3437 = CIRCLE ( 'NONE', #2947, 3.000000000000000888 ) ;
#3438 = CARTESIAN_POINT ( 'NONE',  ( -7.722669826818730404E-14, -20.65026423218563778, -12.51972477286604502 ) ) ;
#3439 = EDGE_LOOP ( 'NONE', ( #3694, #1896, #6611, #14311 ) ) ;
#3440 = EDGE_CURVE ( 'NONE', #8100, #1860, #9992, .T. ) ;
#3441 = CARTESIAN_POINT ( 'NONE',  ( -1.566204647097437563, -6.822536405429463713, -0.8000000000000000444 ) ) ;
#3442 = CARTESIAN_POINT ( 'NONE',  ( 0.08941747217549800286, -14.29395843996395499, 5.279841123860813390 ) ) ;
#3443 = ORIENTED_EDGE ( 'NONE', *, *, #11, .T. ) ;
#3444 = CARTESIAN_POINT ( 'NONE',  ( 59.43001430450886602, 34.23215029930534570, -8.169391093593850073 ) ) ;
#3445 = DIRECTION ( 'NONE',  ( -0.5416238976136773520, 0.8406209333187989463, 0.000000000000000000 ) ) ;
#3446 = B_SPLINE_CURVE_WITH_KNOTS ( 'NONE', 3,
 ( #11947, #14270, #3438, #13022 ),
 .UNSPECIFIED., .F., .F.,
 ( 4, 4 ),
 ( 0.0006045424356928436873, 0.0006887909409525051459 ),
 .UNSPECIFIED. ) ;
#3447 = CARTESIAN_POINT ( 'NONE',  ( 1.749999999999998002, -4.633866840649122132, 27.68468304288257542 ) ) ;
#3448 = DIRECTION ( 'NONE',  ( -0.000000000000000000, -0.000000000000000000, 1.000000000000000000 ) ) ;
#3449 = FACE_OUTER_BOUND ( 'NONE', #3794, .T. ) ;
#3450 = PRODUCT_DEFINITION ( 'UNKNOWN', '', #569, #2861 ) ;
#3451 = EDGE_CURVE ( 'NONE', #14287, #10985, #12033, .T. ) ;
#3452 = EDGE_CURVE ( 'NONE', #11075, #10003, #7830, .T. ) ;
#3453 = CARTESIAN_POINT ( 'NONE',  ( -9.374481487433838394E-15, 2.096460570596369699, -14.05347802000166801 ) ) ;
#3454 = DIRECTION ( 'NONE',  ( -1.000000000000000000, 0.000000000000000000, 0.000000000000000000 ) ) ;
#3455 = ORIENTED_EDGE ( 'NONE', *, *, #15119, .T. ) ;
#3456 = DIRECTION ( 'NONE',  ( 0.000000000000000000, 0.000000000000000000, 1.000000000000000000 ) ) ;
#3457 = DIRECTION ( 'NONE',  ( -0.000000000000000000, 1.000000000000000000, -0.000000000000000000 ) ) ;
#3458 = VERTEX_POINT ( 'NONE', #12433 ) ;
#3459 =( NAMED_UNIT ( * ) SI_UNIT ( $, .STERADIAN. ) SOLID_ANGLE_UNIT ( ) );
#3460 = VERTEX_POINT ( 'NONE', #3221 ) ;
#3461 = VERTEX_POINT ( 'NONE', #12516 ) ;
#3462 = ORIENTED_EDGE ( 'NONE', *, *, #3631, .T. ) ;
#3463 = FACE_BOUND ( 'NONE', #14295, .T. ) ;
#3464 = EDGE_CURVE ( 'NONE', #8188, #11407, #3285, .T. ) ;
#3465 = DIRECTION ( 'NONE',  ( 0.9988110320138940956, 0.04874958797097355551, 0.000000000000000000 ) ) ;
#3466 = CARTESIAN_POINT ( 'NONE',  ( 0.000000000000000000, 0.000000000000000000, -0.8000000000000000444 ) ) ;
#3467 = EDGE_CURVE ( 'NONE', #6106, #3458, #821, .T. ) ;
#3468 = CARTESIAN_POINT ( 'NONE',  ( 2.790000000000000480, -12.51294990530030837, 20.85230829256849105 ) ) ;
#3469 = ORIENTED_EDGE ( 'NONE', *, *, #12340, .T. ) ;
#3470 = LINE ( 'NONE', #14072, #11202 ) ;
#3471 = EDGE_CURVE ( 'NONE', #1149, #1778, #9491, .T. ) ;
#3472 = B_SPLINE_CURVE_WITH_KNOTS ( 'NONE', 3,
 ( #7267, #11939, #1427, #6118, #254, #12021 ),
 .UNSPECIFIED., .F., .F.,
 ( 4, 2, 4 ),
 ( 4.462636678151279571E-07, 0.001879885020955181143, 0.003759323778242547407 ),
 .UNSPECIFIED. ) ;
#3473 = VERTEX_POINT ( 'NONE', #11353 ) ;
#3474 = CARTESIAN_POINT ( 'NONE',  ( 8.961831343790189308, 9.104486995144789319, 6.000000000000000000 ) ) ;
#3475 = CARTESIAN_POINT ( 'NONE',  ( 0.000000000000000000, 0.000000000000000000, 0.000000000000000000 ) ) ;
#3476 = ORIENTED_EDGE ( 'NONE', *, *, #545, .F. ) ;
#3477 = VERTEX_POINT ( 'NONE', #3145 ) ;
#3478 = DIRECTION ( 'NONE',  ( 0.000000000000000000, 0.000000000000000000, -1.000000000000000000 ) ) ;
#3479 = VERTEX_POINT ( 'NONE', #756 ) ;
#3480 = AXIS2_PLACEMENT_3D ( 'NONE', #3220, #2053, #4220 ) ;
#3481 = CARTESIAN_POINT ( 'NONE',  ( 2.021362740937214131, 16.74220655292944926, -5.021526291670140196 ) ) ;
#3482 = DIRECTION ( 'NONE',  ( 0.000000000000000000, 0.000000000000000000, 1.000000000000000000 ) ) ;
#3483 = DIRECTION ( 'NONE',  ( 5.339417856040273846E-17, 1.063174570779084847E-17, -1.000000000000000000 ) ) ;
#3484 = DIRECTION ( 'NONE',  ( -1.000000000000000000, -0.000000000000000000, -0.000000000000000000 ) ) ;
#3485 = APPLICATION_CONTEXT ( 'automotive_design' ) ;
#3486 = EDGE_LOOP ( 'NONE', ( #6728, #10370, #984, #12353, #12284, #1331 ) ) ;
#3487 = CYLINDRICAL_SURFACE ( 'NONE', #916, 13.19999999999999929 ) ;
#3488 = CARTESIAN_POINT ( 'NONE',  ( -9.999999999999998224, 0.000000000000000000, 4.000000000000003553 ) ) ;
#3489 = EDGE_LOOP ( 'NONE', ( #9090, #13919, #13117, #10177, #298, #867, #4996, #9921 ) ) ;
#3490 = AXIS2_PLACEMENT_3D ( 'NONE', #3039, #7727, #13640 ) ;
#3491 = B_SPLINE_CURVE_WITH_KNOTS ( 'NONE', 3,
 ( #9647, #5140, #8719, #13413 ),
 .UNSPECIFIED., .F., .F.,
 ( 4, 4 ),
 ( 0.005258110598983623853, 0.005948376585272730464 ),
 .UNSPECIFIED. ) ;
#3492 = EDGE_LOOP ( 'NONE', ( #9465, #3319, #12934, #6221 ) ) ;
#3493 = CARTESIAN_POINT ( 'NONE',  ( 0.5431871499410860782, -5.154374911959024530, 16.16568790143439571 ) ) ;
#3494 = CARTESIAN_POINT ( 'NONE',  ( 65.21556745095632834, 33.50594455047664866, -2.000000000000000000 ) ) ;
#3495 = DIRECTION ( 'NONE',  ( -0.000000000000000000, -0.000000000000000000, 1.000000000000000000 ) ) ;
#3496 = LINE ( 'NONE', #5822, #6007 ) ;
#3497 = CONTEXT_DEPENDENT_SHAPE_REPRESENTATION ( #7240, #13146 ) ;
#3498 = CARTESIAN_POINT ( 'NONE',  ( 2.031033479673587827, -19.12621924769852555, -19.86422722021333342 ) ) ;
#3499 = EDGE_CURVE ( 'NONE', #14244, #8705, #2134, .T. ) ;
#3500 = CARTESIAN_POINT ( 'NONE',  ( -1.000000000000000222, -4.808326913195983821, -0.8000000000000000444 ) ) ;
#3501 = ORIENTED_EDGE ( 'NONE', *, *, #3197, .T. ) ;
#3503 = VECTOR ( 'NONE', #13162, 1000.000000000000000 ) ;
#3502 = DIRECTION ( 'NONE',  ( -1.000000000000000000, 0.000000000000000000, -0.000000000000000000 ) ) ;
#3504 = CYLINDRICAL_SURFACE ( 'NONE', #7170, 13.19999999999999929 ) ;
#3505 = CARTESIAN_POINT ( 'NONE',  ( 0.02436607992776325046, 16.37294372382858398, 18.55949924794898465 ) ) ;
#3506 = CARTESIAN_POINT ( 'NONE',  ( 2.601776105308176046, -2.857713464478872201, 25.78859396478526733 ) ) ;
#3507 = VERTEX_POINT ( 'NONE', #5529 ) ;
#3508 = VERTEX_POINT ( 'NONE', #978 ) ;
#3509 = EDGE_CURVE ( 'NONE', #7956, #40, #4372, .T. ) ;
#3510 = ORIENTED_EDGE ( 'NONE', *, *, #11921, .F. ) ;
#3511 = DIRECTION ( 'NONE',  ( 0.000000000000000000, 0.000000000000000000, 1.000000000000000000 ) ) ;
#3512 = CARTESIAN_POINT ( 'NONE',  ( -5.999999999999999112, 0.000000000000000000, 3.895000000000000462 ) ) ;
#3513 = ADVANCED_FACE ( 'NONE', ( #3363 ), #1991, .F. ) ;
#3514 = CARTESIAN_POINT ( 'NONE',  ( -19.40394475573012301, -7.794738323547950820, 16.99999999999999645 ) ) ;
#3515 = CARTESIAN_POINT ( 'NONE',  ( 2.582362745529149795, 10.30022894898822727, -12.04200105039459423 ) ) ;
#3516 = CARTESIAN_POINT ( 'NONE',  ( 2.257825459230520693, 4.993157874727810253, 26.58873630738054317 ) ) ;
#3517 = EDGE_CURVE ( 'NONE', #13077, #14623, #6897, .T. ) ;
#3518 = DIRECTION ( 'NONE',  ( 0.000000000000000000, 0.000000000000000000, -1.000000000000000000 ) ) ;
#3519 = LINE ( 'NONE', #122, #5871 ) ;
#3520 = MECHANICAL_DESIGN_GEOMETRIC_PRESENTATION_REPRESENTATION (  '', ( #8429 ), #1598 ) ;
#3521 = VERTEX_POINT ( 'NONE', #897 ) ;
#3522 = CYLINDRICAL_SURFACE ( 'NONE', #1874, 5.999999999999999112 ) ;
#3523 = CARTESIAN_POINT ( 'NONE',  ( 67.23404255319148604, 28.93147646537027384, 4.000000000000003553 ) ) ;
#3524 = EDGE_LOOP ( 'NONE', ( #1049, #5878, #10762, #3898 ) ) ;
#3525 = EDGE_CURVE ( 'NONE', #3993, #3242, #3858, .T. ) ;
#3526 = ORIENTED_EDGE ( 'NONE', *, *, #15119, .F. ) ;
#3527 = VERTEX_POINT ( 'NONE', #10283 ) ;
#3528 = ORIENTED_EDGE ( 'NONE', *, *, #9686, .F. ) ;
#3529 = FACE_BOUND ( 'NONE', #5980, .T. ) ;
#3530 = CARTESIAN_POINT ( 'NONE',  ( 1.749999999999998002, 12.52377138324224148, 25.12109765559658570 ) ) ;
#3531 = CARTESIAN_POINT ( 'NONE',  ( 2.782650468023971868, 14.24968354755765709, -2.217353748341963193 ) ) ;
#3532 = DIRECTION ( 'NONE',  ( -1.000000000000000000, -0.000000000000000000, 0.000000000000000000 ) ) ;
#3533 = AXIS2_PLACEMENT_3D ( 'NONE', #295, #11065, #6154 ) ;
#3534 = EDGE_CURVE ( 'NONE', #99, #2185, #4605, .T. ) ;
#3536 = AXIS2_PLACEMENT_3D ( 'NONE', #10335, #4578, #9398 ) ;
#3535 = CARTESIAN_POINT ( 'NONE',  ( 1.749999999999998002, 0.000000000000000000, 0.000000000000000000 ) ) ;
#3537 = EDGE_LOOP ( 'NONE', ( #5144, #10079, #8328, #13567 ) ) ;
#3538 = CARTESIAN_POINT ( 'NONE',  ( 0.1717365941144614327, -6.008326913195983998, -0.8000000000000000444 ) ) ;
#3539 = EDGE_CURVE ( 'NONE', #6635, #10618, #5457, .T. ) ;
#3540 = CIRCLE ( 'NONE', #12131, 28.06981291497571362 ) ;
#3541 = ADVANCED_FACE ( 'NONE', ( #7749 ), #6821, .T. ) ;
#3542 = VECTOR ( 'NONE', #2175, 1000.000000000000000 ) ;
#3543 = ADVANCED_FACE ( 'NONE', ( #10130 ), #4519, .F. ) ;
#3544 = AXIS2_PLACEMENT_3D ( 'NONE', #13528, #11436, #5401 ) ;
#3545 = ORIENTED_EDGE ( 'NONE', *, *, #8613, .F. ) ;
#3546 = DIRECTION ( 'NONE',  ( -1.000000000000000000, -0.000000000000000000, -0.000000000000000000 ) ) ;
#3547 = CARTESIAN_POINT ( 'NONE',  ( 2.601776144743011443, 23.64332819722380918, 10.68696068830415946 ) ) ;
#3548 = EDGE_LOOP ( 'NONE', ( #4531, #12212, #1113, #2483 ) ) ;
#3549 = ORIENTED_EDGE ( 'NONE', *, *, #6748, .F. ) ;
#3550 = AXIS2_PLACEMENT_3D ( 'NONE', #2595, #14125, #1283 ) ;
#3551 = CARTESIAN_POINT ( 'NONE',  ( 1.387778780781445676E-14, 0.000000000000000000, -7.000000000000007994 ) ) ;
#3552 = AXIS2_PLACEMENT_3D ( 'NONE', #3800, #13014, #10801 ) ;
#3553 = ORIENTED_EDGE ( 'NONE', *, *, #12496, .T. ) ;
#3554 = VECTOR ( 'NONE', #4422, 1000.000000000000000 ) ;
#3555 = FACE_OUTER_BOUND ( 'NONE', #12397, .T. ) ;
#3556 = DIRECTION ( 'NONE',  ( 0.000000000000000000, 0.000000000000000000, 1.000000000000000000 ) ) ;
#3557 = ADVANCED_FACE ( 'NONE', ( #15213 ), #7048, .T. ) ;
#3558 = EDGE_CURVE ( 'NONE', #567, #11124, #3446, .T. ) ;
#3559 = DIRECTION ( 'NONE',  ( -0.9988110320138940956, -0.04874958797097371510, 0.000000000000000000 ) ) ;
#3560 = DIRECTION ( 'NONE',  ( -1.000000000000000000, 0.000000000000000000, 0.000000000000000000 ) ) ;
#3561 = ORIENTED_EDGE ( 'NONE', *, *, #15147, .F. ) ;
#3562 = CARTESIAN_POINT ( 'NONE',  ( 88.46153288930041469, 16.46030115554384565, 2.999999999999999112 ) ) ;
#3563 = ADVANCED_FACE ( 'NONE', ( #1133, #7196 ), #3582, .F. ) ;
#3564 = CARTESIAN_POINT ( 'NONE',  ( -19.40394475573012301, -13.79473832354794993, 14.99999999999999822 ) ) ;
#3565 = EDGE_LOOP ( 'NONE', ( #8398, #13054, #920, #722, #4895, #4828 ) ) ;
#3566 = CIRCLE ( 'NONE', #12883, 17.95481323787947403 ) ;
#3567 = AXIS2_PLACEMENT_3D ( 'NONE', #9388, #11911, #2546 ) ;
#3568 = ORIENTED_EDGE ( 'NONE', *, *, #4269, .T. ) ;
#3569 = CARTESIAN_POINT ( 'NONE',  ( -17.83201772771817772, -12.43434672152745613, -3.799999999999999378 ) ) ;
#3570 = CARTESIAN_POINT ( 'NONE',  ( 31.51081190520435626, 3.030430839836910639, 7.000000000000000000 ) ) ;
#3571 = EDGE_CURVE ( 'NONE', #7839, #8603, #1242, .T. ) ;
#3572 = CARTESIAN_POINT ( 'NONE',  ( 2.508169608347904145, 5.259531939870199402, 15.25429862889483701 ) ) ;
#3573 = CARTESIAN_POINT ( 'NONE',  ( 2.765633920072239071, -16.37294372382844543, -18.55949924794910544 ) ) ;
#3574 = DIRECTION ( 'NONE',  ( 0.000000000000000000, 0.000000000000000000, 1.000000000000000000 ) ) ;
#3575 = LINE ( 'NONE', #4676, #13996 ) ;
#3576 = B_SPLINE_CURVE_WITH_KNOTS ( 'NONE', 3,
 ( #12539, #9089, #938, #8004, #2016, #3179 ),
 .UNSPECIFIED., .F., .F.,
 ( 4, 2, 4 ),
 ( 2.032124546189621919E-07, 0.001878594002992309232, 0.003756984793529999193 ),
 .UNSPECIFIED. ) ;
#3577 = VECTOR ( 'NONE', #1787, 1000.000000000000114 ) ;
#3578 = ORIENTED_EDGE ( 'NONE', *, *, #9884, .F. ) ;
#3579 = CARTESIAN_POINT ( 'NONE',  ( 2.030753610301991419, 19.86438386685660618, 19.12676442129351173 ) ) ;
#3580 = DIRECTION ( 'NONE',  ( 0.000000000000000000, 0.000000000000000000, 1.000000000000000000 ) ) ;
#3581 = DIRECTION ( 'NONE',  ( 0.000000000000000000, 0.000000000000000000, -1.000000000000000000 ) ) ;
#3582 = PLANE ( 'NONE',  #14156 ) ;
#3583 = ORIENTED_EDGE ( 'NONE', *, *, #13023, .T. ) ;
#3584 = ORIENTED_EDGE ( 'NONE', *, *, #3697, .T. ) ;
#3585 = DIRECTION ( 'NONE',  ( 0.000000000000000000, 0.000000000000000000, 1.000000000000000000 ) ) ;
#3586 = ORIENTED_EDGE ( 'NONE', *, *, #3790, .F. ) ;
#3587 = DIRECTION ( 'NONE',  ( 0.000000000000000000, 0.000000000000000000, 1.000000000000000000 ) ) ;
#3588 = CIRCLE ( 'NONE', #7024, 2.524999999999999467 ) ;
#3589 = CARTESIAN_POINT ( 'NONE',  ( 0.000000000000000000, 0.000000000000000000, 3.895000000000000462 ) ) ;
#3590 = LINE ( 'NONE', #2518, #12687 ) ;
#3591 = DIRECTION ( 'NONE',  ( 1.000000000000000000, 0.000000000000000000, 0.000000000000000000 ) ) ;
#3592 = DIRECTION ( 'NONE',  ( -1.576560579138138454E-17, -1.359337748750801300E-17, -0.9999999999999997780 ) ) ;
#3593 = LINE ( 'NONE', #8283, #10375 ) ;
#3594 = ORIENTED_EDGE ( 'NONE', *, *, #14695, .T. ) ;
#3595 = DIRECTION ( 'NONE',  ( 0.000000000000000000, 0.000000000000000000, 1.000000000000000000 ) ) ;
#3596 = CARTESIAN_POINT ( 'NONE',  ( -20.63749999999999929, 4.898587196589412829E-16, 4.000000000000000000 ) ) ;
#3597 = ORIENTED_EDGE ( 'NONE', *, *, #7049, .F. ) ;
#3599 = VECTOR ( 'NONE', #13887, 1000.000000000000000 ) ;
#3598 = DIRECTION ( 'NONE',  ( 0.000000000000000000, 1.000000000000000000, -1.224646799147353207E-16 ) ) ;
#3600 = AXIS2_PLACEMENT_3D ( 'NONE', #7549, #13371, #3936 ) ;
#3601 = CARTESIAN_POINT ( 'NONE',  ( 8.000000000000000000, 0.000000000000000000, 0.000000000000000000 ) ) ;
#3602 = EDGE_CURVE ( 'NONE', #7052, #1632, #13662, .T. ) ;
#3603 = EDGE_LOOP ( 'NONE', ( #3872, #12504, #11780, #15158 ) ) ;
#3604 = AXIS2_PLACEMENT_3D ( 'NONE', #12463, #1080, #5778 ) ;
#3605 = AXIS2_PLACEMENT_3D ( 'NONE', #10744, #2292, #9657 ) ;
#3606 = CARTESIAN_POINT ( 'NONE',  ( 0.000000000000000000, 0.000000000000000000, 0.000000000000000000 ) ) ;
#3607 = ORIENTED_EDGE ( 'NONE', *, *, #14874, .T. ) ;
#3608 = ORIENTED_EDGE ( 'NONE', *, *, #7856, .F. ) ;
#3609 = ORIENTED_EDGE ( 'NONE', *, *, #9159, .T. ) ;
#3610 = FACE_OUTER_BOUND ( 'NONE', #14039, .T. ) ;
#3611 = CARTESIAN_POINT ( 'NONE',  ( 0.000000000000000000, 18.28042085475300382, -15.74360496233363804 ) ) ;
#3612 = VECTOR ( 'NONE', #4581, 1000.000000000000000 ) ;
#3613 = FACE_OUTER_BOUND ( 'NONE', #10521, .T. ) ;
#3614 = DIRECTION ( 'NONE',  ( 0.9021244663126474217, 0.4314758942051349910, -9.480662228539549174E-17 ) ) ;
#3615 = AXIS2_PLACEMENT_3D ( 'NONE', #5465, #4381, #3071 ) ;
#3616 = DIRECTION ( 'NONE',  ( 1.000000000000000000, 0.000000000000000000, 0.000000000000000000 ) ) ;
#3617 = ORIENTED_EDGE ( 'NONE', *, *, #779, .T. ) ;
#3618 = AXIS2_PLACEMENT_3D ( 'NONE', #11876, #271, #10525 ) ;
#3619 = DIRECTION ( 'NONE',  ( -1.000000000000000000, 0.000000000000000000, 0.000000000000000000 ) ) ;
#3620 = AXIS2_PLACEMENT_3D ( 'NONE', #6718, #6415, #11099 ) ;
#3621 = ADVANCED_FACE ( 'NONE', ( #2583 ), #8345, .T. ) ;
#3622 = CIRCLE ( 'NONE', #8783, 10.00000000000000000 ) ;
#3623 = VERTEX_POINT ( 'NONE', #5904 ) ;
#3624 = CARTESIAN_POINT ( 'NONE',  ( 32.66827876307085887, -1.833751565556681173, 4.000000000000000000 ) ) ;
#3625 = DIRECTION ( 'NONE',  ( -0.000000000000000000, -0.000000000000000000, -1.000000000000000000 ) ) ;
#3626 = AXIS2_PLACEMENT_3D ( 'NONE', #13734, #12507, #4279 ) ;
#3627 = ORIENTED_EDGE ( 'NONE', *, *, #10373, .T. ) ;
#3628 = ORIENTED_EDGE ( 'NONE', *, *, #2041, .F. ) ;
#3629 = AXIS2_PLACEMENT_3D ( 'NONE', #11842, #1322, #3706 ) ;
#3630 = DIRECTION ( 'NONE',  ( 0.000000000000000000, 0.000000000000000000, 1.000000000000000000 ) ) ;
#3631 = EDGE_CURVE ( 'NONE', #9813, #6366, #10226, .T. ) ;
#3632 = VERTEX_POINT ( 'NONE', #6968 ) ;
#3633 = ADVANCED_FACE ( 'NONE', ( #6125 ), #13095, .F. ) ;
#3634 = DIRECTION ( 'NONE',  ( 0.9728364810787193395, 0.2314933715733012431, 0.000000000000000000 ) ) ;
#3635 = B_SPLINE_CURVE_WITH_KNOTS ( 'NONE', 3,
 ( #8551, #14320, #10928, #13310, #2786, #7481 ),
 .UNSPECIFIED., .F., .F.,
 ( 4, 2, 4 ),
 ( 2.132675795041204291E-07, 0.001878604073277003036, 0.003756994878974502169 ),
 .UNSPECIFIED. ) ;
#3636 = CARTESIAN_POINT ( 'NONE',  ( 2.789999999999999147, -5.249430348645663713, -12.98979500319699731 ) ) ;
#3637 = CARTESIAN_POINT ( 'NONE',  ( 0.0003207540509378258692, 20.70663861606293921, -12.51925356660738053 ) ) ;
#3638 = CARTESIAN_POINT ( 'NONE',  ( -0.1713913650100259145, 0.000000000000000000, 0.000000000000000000 ) ) ;
#3639 = VECTOR ( 'NONE', #5430, 1000.000000000000000 ) ;
#3640 = ORIENTED_EDGE ( 'NONE', *, *, #10599, .F. ) ;
#3641 = AXIS2_PLACEMENT_3D ( 'NONE', #11261, #6655, #735 ) ;
#3642 = PLANE ( 'NONE',  #6807 ) ;
#3643 = CARTESIAN_POINT ( 'NONE',  ( -19.40394475573012301, -13.79473832354794993, 14.99999999999999822 ) ) ;
#3644 = VERTEX_POINT ( 'NONE', #4603 ) ;
#3645 = ORIENTED_EDGE ( 'NONE', *, *, #5172, .F. ) ;
#3646 = ORIENTED_EDGE ( 'NONE', *, *, #2231, .F. ) ;
#3647 = EDGE_CURVE ( 'NONE', #8611, #10625, #12186, .T. ) ;
#3648 = FACE_BOUND ( 'NONE', #287, .T. ) ;
#3649 = CARTESIAN_POINT ( 'NONE',  ( 0.000000000000000000, 0.4273491293402468805, 0.000000000000000000 ) ) ;
#3650 = ADVANCED_FACE ( 'NONE', ( #7124 ), #8126, .F. ) ;
#3651 = CARTESIAN_POINT ( 'NONE',  ( -0.1085714285714285687, -3.798448662927795372, -0.8000000000000000444 ) ) ;
#3652 = DIRECTION ( 'NONE',  ( -0.000000000000000000, -0.000000000000000000, 1.000000000000000000 ) ) ;
#3653 = ITEM_DEFINED_TRANSFORMATION ( 'NONE', 'NONE', #12138,  #1376 ) ;
#3655 = VECTOR ( 'NONE', #14978, 1000.000000000000000 ) ;
#3654 = DIRECTION ( 'NONE',  ( 0.000000000000000000, 0.000000000000000000, 1.000000000000000000 ) ) ;
#3656 = ADVANCED_FACE ( 'NONE', ( #2509 ), #1274, .T. ) ;
#3657 = CARTESIAN_POINT ( 'NONE',  ( 2.010451919658888809, 4.029281904976634188, 16.99607982911243198 ) ) ;
#3658 = ORIENTED_EDGE ( 'NONE', *, *, #505, .F. ) ;
#3659 = DIRECTION ( 'NONE',  ( -1.000000000000000000, -0.000000000000000000, -0.000000000000000000 ) ) ;
#3660 = DIRECTION ( 'NONE',  ( 0.000000000000000000, 0.000000000000000000, 1.000000000000000000 ) ) ;
#3661 = DIRECTION ( 'NONE',  ( -1.000000000000000000, -0.000000000000000000, 0.000000000000000000 ) ) ;
#3662 = DIRECTION ( 'NONE',  ( -1.000000000000000000, -0.000000000000000000, -0.000000000000000000 ) ) ;
#3663 = EDGE_CURVE ( 'NONE', #13730, #626, #6004, .T. ) ;
#3664 = VERTEX_POINT ( 'NONE', #10651 ) ;
#3665 = AXIS2_PLACEMENT_3D ( 'NONE', #11460, #9238, #5562 ) ;
#3666 = ORIENTED_EDGE ( 'NONE', *, *, #2442, .F. ) ;
#3667 = ORIENTED_EDGE ( 'NONE', *, *, #10596, .T. ) ;
#3668 = CARTESIAN_POINT ( 'NONE',  ( 0.5431870686475177568, 11.42270873787292551, 12.54666350726128243 ) ) ;
#3669 = CARTESIAN_POINT ( 'NONE',  ( 1.749999999999998002, -19.67366047555545094, 20.02152543075338187 ) ) ;
#3670 = CARTESIAN_POINT ( 'NONE',  ( 1.398397006336996817, -6.091550361990593743, 0.000000000000000000 ) ) ;
#3671 = CARTESIAN_POINT ( 'NONE',  ( 1.749999999999999778, 12.55714665600005020, -12.83329210556818545 ) ) ;
#3672 = CARTESIAN_POINT ( 'NONE',  ( 0.000000000000000000, 0.000000000000000000, 0.000000000000000000 ) ) ;
#3673 = DIRECTION ( 'NONE',  ( 0.000000000000000000, -0.9510565162951523099, -0.3090169943749515591 ) ) ;
#3674 = EDGE_LOOP ( 'NONE', ( #3766, #7349, #5852, #11321, #11991, #9247 ) ) ;
#3675 = FACE_OUTER_BOUND ( 'NONE', #4958, .T. ) ;
#3676 = DIRECTION ( 'NONE',  ( 0.9863939238321436376, 0.1643989873053573192, 0.000000000000000000 ) ) ;
#3677 = AXIS2_PLACEMENT_3D ( 'NONE', #12196, #2753, #6286 ) ;
#3678 = ORIENTED_EDGE ( 'NONE', *, *, #13035, .T. ) ;
#3679 = DIRECTION ( 'NONE',  ( -1.000000000000000000, -0.000000000000000000, -0.000000000000000000 ) ) ;
#3680 = FACE_BOUND ( 'NONE', #3239, .T. ) ;
#3681 = DIRECTION ( 'NONE',  ( 1.000000000000000000, 0.000000000000000000, 0.000000000000000000 ) ) ;
#3682 = EDGE_LOOP ( 'NONE', ( #8348, #1401, #8006, #12251 ) ) ;
#3683 = VERTEX_POINT ( 'NONE', #9504 ) ;
#3684 = ORIENTED_EDGE ( 'NONE', *, *, #5847, .T. ) ;
#3685 = ORIENTED_EDGE ( 'NONE', *, *, #840, .T. ) ;
#3686 = CARTESIAN_POINT ( 'NONE',  ( -7.664413047240269201E-14, 2.133839912090805147, 24.22524813288763568 ) ) ;
#3687 = CARTESIAN_POINT ( 'NONE',  ( 0.07473579423048609671, 15.04916547791954606, 2.569134216958950834 ) ) ;
#3688 = DIRECTION ( 'NONE',  ( -5.480158469902917989E-17, -1.051478716308701742E-16, -1.000000000000000000 ) ) ;
#3689 = B_SPLINE_CURVE_WITH_KNOTS ( 'NONE', 3,
 ( #4833, #14122, #10659, #4918 ),
 .UNSPECIFIED., .F., .F.,
 ( 4, 4 ),
 ( 1.981826382900847025E-07, 0.0006887856082032273912 ),
 .UNSPECIFIED. ) ;
#3690 = CARTESIAN_POINT ( 'NONE',  ( 0.9041604829517128072, -4.239993951493329583, 17.20101185193998106 ) ) ;
#3691 = EDGE_CURVE ( 'NONE', #929, #6042, #7779, .T. ) ;
#3692 = ORIENTED_EDGE ( 'NONE', *, *, #6049, .F. ) ;
#3693 = CARTESIAN_POINT ( 'NONE',  ( 31.51081190520435626, 3.030430839836910639, -2.000000000000000888 ) ) ;
#3694 = ORIENTED_EDGE ( 'NONE', *, *, #12813, .F. ) ;
#3695 = CARTESIAN_POINT ( 'NONE',  ( 0.02436607992775717893, -9.836394144775869819, 22.71065055754449347 ) ) ;
#3696 = PRODUCT_DEFINITION_SHAPE ( 'NONE', 'NONE',  #15236 ) ;
#3697 = EDGE_CURVE ( 'NONE', #10279, #3235, #6197, .T. ) ;
#3698 = CARTESIAN_POINT ( 'NONE',  ( 2.765633920072235963, 22.71065055754452544, 9.836394144775786330 ) ) ;
#3699 = ORIENTED_EDGE ( 'NONE', *, *, #5310, .T. ) ;
#3700 = VERTEX_POINT ( 'NONE', #4129 ) ;
#3701 = EDGE_CURVE ( 'NONE', #10080, #14810, #10956, .T. ) ;
#3702 = DIRECTION ( 'NONE',  ( 0.000000000000000000, 0.000000000000000000, 1.000000000000000000 ) ) ;
#3703 = ORIENTED_EDGE ( 'NONE', *, *, #10759, .T. ) ;
#3704 = CARTESIAN_POINT ( 'NONE',  ( 2.789999999999999147, -4.595504208220129172, 14.19996452731187553 ) ) ;
#3705 = EDGE_CURVE ( 'NONE', #4798, #8127, #148, .T. ) ;
#3706 = DIRECTION ( 'NONE',  ( 0.000000000000000000, 0.000000000000000000, 1.000000000000000000 ) ) ;
#3707 = DIRECTION ( 'NONE',  ( -1.000000000000000000, 0.000000000000000000, 0.000000000000000000 ) ) ;
#3708 = CARTESIAN_POINT ( 'NONE',  ( -3.160591952521660364, -3.281206521718067037, -0.8000000000000000444 ) ) ;
#3709 = VERTEX_POINT ( 'NONE', #11035 ) ;
#3710 = DIRECTION ( 'NONE',  ( 1.000000000000000000, 0.000000000000000000, 0.000000000000000000 ) ) ;
#3711 = B_SPLINE_CURVE_WITH_KNOTS ( 'NONE', 3,
 ( #10055, #11697, #10485, #4657 ),
 .UNSPECIFIED., .F., .F.,
 ( 4, 4 ),
 ( 0.005258214619651972732, 0.005948481662034169060 ),
 .UNSPECIFIED. ) ;
#3712 = CARTESIAN_POINT ( 'NONE',  ( 0.02436607992775674525, 9.836394144776026138, -22.71065055754441531 ) ) ;
#3713 = VERTEX_POINT ( 'NONE', #1739 ) ;
#3714 = DIRECTION ( 'NONE',  ( -0.000000000000000000, -0.000000000000000000, -1.000000000000000000 ) ) ;
#3715 = EDGE_CURVE ( 'NONE', #8611, #5631, #12334, .T. ) ;
#3716 = EDGE_CURVE ( 'NONE', #5643, #6579, #13714, .T. ) ;
#3717 = MANIFOLD_SOLID_BREP ( 'Mirror2', #571 ) ;
#3718 = ORIENTED_EDGE ( 'NONE', *, *, #12246, .T. ) ;
#3719 = ORIENTED_EDGE ( 'NONE', *, *, #12615, .T. ) ;
#3720 = CARTESIAN_POINT ( 'NONE',  ( 2.790000000000007585, 8.842327429719095022, 11.12243880662616569 ) ) ;
#3721 = CARTESIAN_POINT ( 'NONE',  ( -1.906188514513426096E-16, -24.22479935914659066, -2.133490293297270579 ) ) ;
#3722 = CIRCLE ( 'NONE', #12313, 17.95481323787947758 ) ;
#3723 = CARTESIAN_POINT ( 'NONE',  ( 1.039999999999997593, 0.000000000000000000, 0.000000000000000000 ) ) ;
#3724 = DIRECTION ( 'NONE',  ( 1.000000000000000000, 0.000000000000000000, 0.000000000000000000 ) ) ;
#3725 = CARTESIAN_POINT ( 'NONE',  ( 2.789999999999999147, 25.59481291497571220, 0.000000000000000000 ) ) ;
#3726 = LINE ( 'NONE', #11029, #10256 ) ;
#3727 = ORIENTED_EDGE ( 'NONE', *, *, #1057, .F. ) ;
#3728 = FACE_OUTER_BOUND ( 'NONE', #3813, .T. ) ;
#3729 = DIRECTION ( 'NONE',  ( -1.000000000000000000, -0.000000000000000000, -0.000000000000000000 ) ) ;
#3730 = CYLINDRICAL_SURFACE ( 'NONE', #8311, 13.20000000000000284 ) ;
#3731 = DIRECTION ( 'NONE',  ( 0.000000000000000000, 0.000000000000000000, 1.000000000000000000 ) ) ;
#3732 = ADVANCED_FACE ( 'NONE', ( #2670 ), #8493, .T. ) ;
#3733 = AXIS2_PLACEMENT_3D ( 'NONE', #2072, #769, #6763 ) ;
#3734 = CIRCLE ( 'NONE', #4980, 4.999999999999997335 ) ;
#3735 = VERTEX_POINT ( 'NONE', #2966 ) ;
#3736 = VERTEX_POINT ( 'NONE', #1810 ) ;
#3737 = EDGE_CURVE ( 'NONE', #8554, #12755, #661, .T. ) ;
#3738 = EDGE_CURVE ( 'NONE', #1885, #13883, #4978, .T. ) ;
#3739 = ORIENTED_EDGE ( 'NONE', *, *, #1654, .T. ) ;
#3740 = CARTESIAN_POINT ( 'NONE',  ( 2.790000000000000924, 4.898587196589412829E-16, -4.000000000000000000 ) ) ;
#3741 = CARTESIAN_POINT ( 'NONE',  ( 93.49175023922396122, 0.6585002008270834928, -2.000000000000000888 ) ) ;
#3742 = LINE ( 'NONE', #7060, #3865 ) ;
#3743 = CARTESIAN_POINT ( 'NONE',  ( 0.7589665349472695111, -27.14933624560910630, 4.828387785247921116 ) ) ;
#3744 = DIRECTION ( 'NONE',  ( 0.000000000000000000, 0.000000000000000000, 1.000000000000000000 ) ) ;
#3745 = DIRECTION ( 'NONE',  ( -1.000000000000000000, 0.000000000000000000, 0.000000000000000000 ) ) ;
#3746 = ORIENTED_EDGE ( 'NONE', *, *, #12567, .F. ) ;
#3747 = CARTESIAN_POINT ( 'NONE',  ( 0.000000000000000000, 0.000000000000000000, 4.500000000000000888 ) ) ;
#3748 = DIRECTION ( 'NONE',  ( 0.000000000000000000, 0.000000000000000000, 1.000000000000000000 ) ) ;
#3749 = ORIENTED_EDGE ( 'NONE', *, *, #3084, .T. ) ;
#3750 = LINE ( 'NONE', #2176, #4379 ) ;
#3751 = CARTESIAN_POINT ( 'NONE',  ( 0.5537796877189875566, 11.41743294611093340, -12.52687487503407127 ) ) ;
#3752 = CIRCLE ( 'NONE', #4749, 4.000000000000000000 ) ;
#3753 = CARTESIAN_POINT ( 'NONE',  ( 93.49175023922396122, 0.6585002008270834928, 7.000000000000000000 ) ) ;
#3754 = ORIENTED_EDGE ( 'NONE', *, *, #11799, .T. ) ;
#3755 =( LENGTH_UNIT ( ) NAMED_UNIT ( * ) SI_UNIT ( .MILLI., .METRE. ) );
#3756 = ORIENTED_EDGE ( 'NONE', *, *, #5136, .T. ) ;
#3757 = VERTEX_POINT ( 'NONE', #14345 ) ;
#3758 = ORIENTED_EDGE ( 'NONE', *, *, #9652, .F. ) ;
#3759 = DIRECTION ( 'NONE',  ( 0.000000000000000000, 0.000000000000000000, 1.000000000000000000 ) ) ;
#3760 = LINE ( 'NONE', #12981, #13183 ) ;
#3761 = DIRECTION ( 'NONE',  ( -0.9148936170212769170, -0.4036950204470262649, 0.000000000000000000 ) ) ;
#3762 = CARTESIAN_POINT ( 'NONE',  ( 86.17559721729969624, 12.01344854909570259, -2.000000000000000888 ) ) ;
#3763 = DIRECTION ( 'NONE',  ( -0.9988110320138940956, -0.04874958797097371510, -0.000000000000000000 ) ) ;
#3764 = ADVANCED_FACE ( 'NONE', ( #5141 ), #9812, .T. ) ;
#3765 = CARTESIAN_POINT ( 'NONE',  ( 2.508169719062757430, 12.18203740414267244, 10.58084377126627018 ) ) ;
#3766 = ORIENTED_EDGE ( 'NONE', *, *, #9932, .F. ) ;
#3767 = CARTESIAN_POINT ( 'NONE',  ( 0.000000000000000000, 12.52067188844351442, 20.62201879784919001 ) ) ;
#3768 = ORIENTED_EDGE ( 'NONE', *, *, #3111, .T. ) ;
#3769 = ORIENTED_EDGE ( 'NONE', *, *, #3274, .F. ) ;
#3770 = CARTESIAN_POINT ( 'NONE',  ( 1.150000000000000577, 7.225416114969384193E-16, 5.899999999999999467 ) ) ;
#3771 = DIRECTION ( 'NONE',  ( 0.9914448613738103822, -0.1305261922200521840, 0.000000000000000000 ) ) ;
#3772 = EDGE_CURVE ( 'NONE', #7850, #8078, #9673, .T. ) ;
#3773 = ORIENTED_EDGE ( 'NONE', *, *, #3325, .T. ) ;
#3774 = VECTOR ( 'NONE', #14090, 1000.000000000000000 ) ;
#3775 = ORIENTED_EDGE ( 'NONE', *, *, #12835, .T. ) ;
#3776 = AXIS2_PLACEMENT_3D ( 'NONE', #7622, #14248, #7254 ) ;
#3777 = AXIS2_PLACEMENT_3D ( 'NONE', #14750, #1908, #13579 ) ;
#3778 = CYLINDRICAL_SURFACE ( 'NONE', #625, 17.95481323787947403 ) ;
#3779 = ORIENTED_EDGE ( 'NONE', *, *, #4004, .T. ) ;
#3780 = LINE ( 'NONE', #1486, #4029 ) ;
#3781 = DIRECTION ( 'NONE',  ( -0.4571871344001416926, -0.8893705212896291235, 0.000000000000000000 ) ) ;
#3782 = CIRCLE ( 'NONE', #4789, 2.524999999999996803 ) ;
#3783 = ADVANCED_FACE ( 'NONE', ( #7508 ), #1665, .T. ) ;
#3784 = CARTESIAN_POINT ( 'NONE',  ( 2.783068930044318545, 16.17493693894878604, 18.43696893154764282 ) ) ;
#3785 = CARTESIAN_POINT ( 'NONE',  ( 98.48580539929344013, 0.9022481406819604643, 7.000000000000000000 ) ) ;
#3786 = AXIS2_PLACEMENT_3D ( 'NONE', #1699, #1622, #375 ) ;
#3787 = PRESENTATION_LAYER_ASSIGNMENT (  '', '', ( #5037 ) ) ;
#3788 = ORIENTED_EDGE ( 'NONE', *, *, #13787, .T. ) ;
#3789 = DIRECTION ( 'NONE',  ( 0.1643989873053573469, -0.9863939238321437486, 0.000000000000000000 ) ) ;
#3790 = EDGE_CURVE ( 'NONE', #9602, #11452, #7050, .T. ) ;
#3791 = DIRECTION ( 'NONE',  ( -1.000000000000000000, 0.000000000000000000, 0.000000000000000000 ) ) ;
#3792 = VERTEX_POINT ( 'NONE', #5509 ) ;
#3793 = CARTESIAN_POINT ( 'NONE',  ( -16.23224367729419271, -7.237025146040845236, -3.000000000000000444 ) ) ;
#3794 = EDGE_LOOP ( 'NONE', ( #9268, #11771, #5483, #14494 ) ) ;
#3795 = ORIENTED_EDGE ( 'NONE', *, *, #14182, .F. ) ;
#3796 = FACE_BOUND ( 'NONE', #14928, .T. ) ;
#3798 = CYLINDRICAL_SURFACE ( 'NONE', #1188, 4.000000000000000888 ) ;
#3797 = CIRCLE ( 'NONE', #5048, 4.000000000000000888 ) ;
#3799 = MECHANICAL_DESIGN_GEOMETRIC_PRESENTATION_REPRESENTATION (  '', ( #15102 ), #616 ) ;
#3800 = CARTESIAN_POINT ( 'NONE',  ( 80.82762530298222714, -19.99999999999999645, 7.000000000000006217 ) ) ;
#3801 = CONTEXT_DEPENDENT_SHAPE_REPRESENTATION ( #9690, #7145 ) ;
#3802 = CARTESIAN_POINT ( 'NONE',  ( 0.000000000000000000, -1.948757464274271767, 13.87420763704360915 ) ) ;
#3803 = DIRECTION ( 'NONE',  ( 0.000000000000000000, 0.000000000000000000, 1.000000000000000000 ) ) ;
#3804 = ORIENTED_EDGE ( 'NONE', *, *, #14274, .F. ) ;
#3805 = DIRECTION ( 'NONE',  ( 0.000000000000000000, 0.000000000000000000, -1.000000000000000000 ) ) ;
#3806 = CARTESIAN_POINT ( 'NONE',  ( 0.02436607992776238310, -2.336989772644097574, -24.63872515616085224 ) ) ;
#3807 = DIRECTION ( 'NONE',  ( -1.000000000000000000, -0.000000000000000000, -0.000000000000000000 ) ) ;
#3808 = AXIS2_PLACEMENT_3D ( 'NONE', #9493, #8260, #8404 ) ;
#3809 = CARTESIAN_POINT ( 'NONE',  ( 0.006974771092478231072, 9.686319561460942751, 22.53337530003406997 ) ) ;
#3810 = CIRCLE ( 'NONE', #15113, 2.999999999999988898 ) ;
#3811 = ORIENTED_EDGE ( 'NONE', *, *, #4323, .T. ) ;
#3812 = CIRCLE ( 'NONE', #6519, 28.06981291497571362 ) ;
#3813 = EDGE_LOOP ( 'NONE', ( #12460, #13499, #4147, #618, #1610, #12136, #15055, #4610 ) ) ;
#3814 = EDGE_CURVE ( 'NONE', #154, #6827, #9014, .T. ) ;
#3815 = ORIENTED_EDGE ( 'NONE', *, *, #5807, .T. ) ;
#3816 = LINE ( 'NONE', #12031, #2637 ) ;
#3817 = CARTESIAN_POINT ( 'NONE',  ( 0.7589665089996505687, 12.05173163741758380, -24.80232951178364686 ) ) ;
#3818 = CARTESIAN_POINT ( 'NONE',  ( 0.000000000000000000, 0.000000000000000000, 7.799999999999990052 ) ) ;
#3819 = CARTESIAN_POINT ( 'NONE',  ( 0.02531912748464674665, 11.36963888406700285, -9.232963481057645083 ) ) ;
#3820 = DIRECTION ( 'NONE',  ( -0.7573544145849103737, -0.6530040510661074826, 2.081668171172168205E-17 ) ) ;
#3821 = FACE_OUTER_BOUND ( 'NONE', #9441, .T. ) ;
#3822 = MANIFOLD_SOLID_BREP ( 'Cut-Extrude5', #9667 ) ;
#3823 = EDGE_LOOP ( 'NONE', ( #52, #4946 ) ) ;
#3824 = DIRECTION ( 'NONE',  ( 0.000000000000000000, 0.000000000000000000, 1.000000000000000000 ) ) ;
#3825 = CARTESIAN_POINT ( 'NONE',  ( 8.000000000000000000, 0.000000000000000000, 0.000000000000000000 ) ) ;
#3826 = EDGE_CURVE ( 'NONE', #14563, #8616, #3130, .T. ) ;
#3827 = EDGE_CURVE ( 'NONE', #5429, #3757, #6658, .T. ) ;
#3828 = ORIENTED_EDGE ( 'NONE', *, *, #11609, .T. ) ;
#3829 = CARTESIAN_POINT ( 'NONE',  ( -16.92833982302709828, -13.89754826684236200, -3.471826001292096363E-15 ) ) ;
#3830 = CARTESIAN_POINT ( 'NONE',  ( 1.749999999999998002, 24.89775460606832524, 12.96210679857795256 ) ) ;
#3831 = B_SPLINE_CURVE_WITH_KNOTS ( 'NONE', 3,
 ( #6342, #5434, #13490, #10104 ),
 .UNSPECIFIED., .F., .F.,
 ( 4, 4 ),
 ( 0.005123695899043907188, 0.005814329666474870977 ),
 .UNSPECIFIED. ) ;
#3832 = DIRECTION ( 'NONE',  ( -5.480158469902919838E-17, -1.051478716308701618E-16, -1.000000000000000000 ) ) ;
#3833 = VECTOR ( 'NONE', #10303, 1000.000000000000000 ) ;
#3834 = ORIENTED_EDGE ( 'NONE', *, *, #13026, .T. ) ;
#3835 = AXIS2_PLACEMENT_3D ( 'NONE', #13891, #12733, #6900 ) ;
#3836 = CARTESIAN_POINT ( 'NONE',  ( 0.2818302809372404405, -12.18203740414274705, 10.58084377126619025 ) ) ;
#3837 = CARTESIAN_POINT ( 'NONE',  ( 0.2818303507154734100, -15.84037596932109615, 3.072260951847473720 ) ) ;
#3838 = VERTEX_POINT ( 'NONE', #1895 ) ;
#3839 = ORIENTED_EDGE ( 'NONE', *, *, #11668, .F. ) ;
#3840 = ORIENTED_EDGE ( 'NONE', *, *, #11861, .T. ) ;
#3841 = CARTESIAN_POINT ( 'NONE',  ( 13.78117670802322259, -24.07785181381190753, 2.000000000000000000 ) ) ;
#3842 = DIRECTION ( 'NONE',  ( 1.000000000000000000, 0.000000000000000000, 0.000000000000000000 ) ) ;
#3843 = DIRECTION ( 'NONE',  ( 0.1643989873053574580, -0.9863939238321436376, 0.000000000000000000 ) ) ;
#3844 = DIRECTION ( 'NONE',  ( 0.000000000000000000, 0.000000000000000000, 1.000000000000000000 ) ) ;
#3845 = EDGE_CURVE ( 'NONE', #626, #3410, #492, .T. ) ;
#3846 = FACE_OUTER_BOUND ( 'NONE', #12933, .T. ) ;
#3847 = EDGE_CURVE ( 'NONE', #4705, #10796, #9481, .T. ) ;
#3848 = AXIS2_PLACEMENT_3D ( 'NONE', #8269, #13972, #11649 ) ;
#3849 = AXIS2_PLACEMENT_3D ( 'NONE', #4003, #8674, #5099 ) ;
#3850 = DIRECTION ( 'NONE',  ( 0.000000000000000000, 0.000000000000000000, 1.000000000000000000 ) ) ;
#3851 = ADVANCED_FACE ( 'NONE', ( #4502 ), #7950, .F. ) ;
#3852 = EDGE_LOOP ( 'NONE', ( #9445, #13967, #50, #8954 ) ) ;
#3853 = FACE_OUTER_BOUND ( 'NONE', #6301, .T. ) ;
#3854 = VECTOR ( 'NONE', #11897, 1000.000000000000000 ) ;
#3855 = VECTOR ( 'NONE', #2357, 1000.000000000000114 ) ;
#3856 = ADVANCED_FACE ( 'NONE', ( #2038 ), #8032, .F. ) ;
#3857 =( NAMED_UNIT ( * ) SI_UNIT ( $, .STERADIAN. ) SOLID_ANGLE_UNIT ( ) );
#3858 = CIRCLE ( 'NONE', #11937, 6.000000000000000888 ) ;
#3859 = B_SPLINE_CURVE_WITH_KNOTS ( 'NONE', 3,
 ( #1165, #12828, #15078, #6648 ),
 .UNSPECIFIED., .F., .F.,
 ( 4, 4 ),
 ( 4.462636695580848051E-07, 0.0004963285629697519611 ),
 .UNSPECIFIED. ) ;
#3860 = ORIENTED_EDGE ( 'NONE', *, *, #4513, .T. ) ;
#3861 = VERTEX_POINT ( 'NONE', #14968 ) ;
#3862 = DIRECTION ( 'NONE',  ( 0.000000000000000000, 1.224646799147351975E-16, 1.000000000000000000 ) ) ;
#3863 = CARTESIAN_POINT ( 'NONE',  ( 1.039999999999996927, -4.633866840649124796, 27.68468304288256832 ) ) ;
#3864 = ORIENTED_EDGE ( 'NONE', *, *, #4204, .T. ) ;
#3865 = VECTOR ( 'NONE', #11805, 1000.000000000000000 ) ;
#3866 = AXIS2_PLACEMENT_3D ( 'NONE', #7153, #14378, #102 ) ;
#3867 = CARTESIAN_POINT ( 'NONE',  ( -0.1085714285714285687, -3.798448662927795372, 0.000000000000000000 ) ) ;
#3868 = ORIENTED_EDGE ( 'NONE', *, *, #3317, .T. ) ;
#3869 = CARTESIAN_POINT ( 'NONE',  ( 69.97572749000833880, 15.55805301486455683, -2.000000000000000888 ) ) ;
#3870 = DIRECTION ( 'NONE',  ( 0.000000000000000000, 0.000000000000000000, 1.000000000000000000 ) ) ;
#3871 = CARTESIAN_POINT ( 'NONE',  ( 0.5321745379877897975, 12.96514671151801323, -23.74442027961346113 ) ) ;
#3872 = ORIENTED_EDGE ( 'NONE', *, *, #4677, .T. ) ;
#3873 =( GEOMETRIC_REPRESENTATION_CONTEXT ( 3 ) GLOBAL_UNCERTAINTY_ASSIGNED_CONTEXT ( ( #5339 ) ) GLOBAL_UNIT_ASSIGNED_CONTEXT ( ( #10257, #9104, #5577 ) ) REPRESENTATION_CONTEXT ( 'NONE', 'WORKASPACE' ) );
#3874 = DIRECTION ( 'NONE',  ( -1.000000000000000000, 0.000000000000000000, 0.000000000000000000 ) ) ;
#3875 = PLANE ( 'NONE',  #2862 ) ;
#3876 = AXIS2_PLACEMENT_3D ( 'NONE', #3975, #1514, #1591 ) ;
#3877 = AXIS2_PLACEMENT_3D ( 'NONE', #14635, #3103, #11155 ) ;
#3878 = EDGE_CURVE ( 'NONE', #14446, #5284, #7729, .T. ) ;
#3879 = ORIENTED_EDGE ( 'NONE', *, *, #10879, .T. ) ;
#3880 = DIRECTION ( 'NONE',  ( 1.000000000000000000, 0.000000000000000000, 0.000000000000000000 ) ) ;
#3881 = CARTESIAN_POINT ( 'NONE',  ( 0.1713913650100259145, 0.000000000000000000, 0.000000000000000000 ) ) ;
#3882 = ORIENTED_EDGE ( 'NONE', *, *, #4195, .T. ) ;
#3883 = ORIENTED_EDGE ( 'NONE', *, *, #11255, .F. ) ;
#3884 = FACE_BOUND ( 'NONE', #2709, .T. ) ;
#3885 = AXIS2_PLACEMENT_3D ( 'NONE', #12740, #13675, #5467 ) ;
#3886 =( LENGTH_UNIT ( ) NAMED_UNIT ( * ) SI_UNIT ( .MILLI., .METRE. ) );
#3887 = FACE_BOUND ( 'NONE', #11709, .T. ) ;
#3888 = CONTEXT_DEPENDENT_SHAPE_REPRESENTATION ( #8025, #4445 ) ;
#3889 = CARTESIAN_POINT ( 'NONE',  ( 2.765633920072241292, 18.55949924794916228, -16.37294372382838148 ) ) ;
#3890 = CIRCLE ( 'NONE', #6594, 2.999999999999975131 ) ;
#3891 = AXIS2_PLACEMENT_3D ( 'NONE', #14427, #3893, #9874 ) ;
#3892 = ORIENTED_EDGE ( 'NONE', *, *, #9551, .F. ) ;
#3893 = DIRECTION ( 'NONE',  ( -1.000000000000000000, -2.081668171172168513E-16, 0.000000000000000000 ) ) ;
#3894 = DIRECTION ( 'NONE',  ( 0.1643989873053578465, -0.9863939238321436376, 0.000000000000000000 ) ) ;
#3895 = CARTESIAN_POINT ( 'NONE',  ( 2.789999999999999147, -14.18181402625756959, 19.91106274590508107 ) ) ;
#3896 = DIRECTION ( 'NONE',  ( 0.5416238976136762417, -0.8406209333187997235, 0.000000000000000000 ) ) ;
#3897 = ORIENTED_EDGE ( 'NONE', *, *, #8754, .T. ) ;
#3898 = ORIENTED_EDGE ( 'NONE', *, *, #7500, .F. ) ;
#3899 = ORIENTED_EDGE ( 'NONE', *, *, #8713, .T. ) ;
#3900 = APPLICATION_CONTEXT ( 'automotive_design' ) ;
#3901 = TOROIDAL_SURFACE ( 'NONE', #8810, 4.100000000000000533, 0.1000000000000001582 ) ;
#3902 = AXIS2_PLACEMENT_3D ( 'NONE', #9807, #9725, #1430 ) ;
#3903 = CARTESIAN_POINT ( 'NONE',  ( 0.7592463965288811512, -24.32906614999605921, -12.98165646470108925 ) ) ;
#3904 = VECTOR ( 'NONE', #15045, 1000.000000000000000 ) ;
#3905 = DIRECTION ( 'NONE',  ( 1.000000000000000000, 0.000000000000000000, 0.000000000000000000 ) ) ;
#3906 = DIRECTION ( 'NONE',  ( 1.000000000000000000, 0.000000000000000000, 0.000000000000000000 ) ) ;
#3907 = DIRECTION ( 'NONE',  ( -1.000000000000000000, -0.000000000000000000, -0.000000000000000000 ) ) ;
#3908 = CARTESIAN_POINT ( 'NONE',  ( 80.00000000000001421, 1.084202172485504434E-16, 0.1050000000000009259 ) ) ;
#3909 = CARTESIAN_POINT ( 'NONE',  ( 2.560885596921109730, 15.06658931286051839, 5.279841123860919971 ) ) ;
#3910 = EDGE_CURVE ( 'NONE', #1519, #5234, #9115, .T. ) ;
#3911 = EDGE_LOOP ( 'NONE', ( #14581, #3667, #5796, #6423 ) ) ;
#3912 = CARTESIAN_POINT ( 'NONE',  ( 1.960886852992497653, -24.44424927289185590, 12.96989951879399072 ) ) ;
#3913 = FACE_OUTER_BOUND ( 'NONE', #13789, .T. ) ;
#3914 = EDGE_LOOP ( 'NONE', ( #1707, #2916, #11211, #3307 ) ) ;
#3915 = CARTESIAN_POINT ( 'NONE',  ( 0.006931111373679591826, -22.53293026234497276, -9.685942809247297447 ) ) ;
#3916 = DIRECTION ( 'NONE',  ( 1.000000000000000000, 0.000000000000000000, 0.000000000000000000 ) ) ;
#3917 = EDGE_CURVE ( 'NONE', #269, #447, #12920, .T. ) ;
#3918 = AXIS2_PLACEMENT_3D ( 'NONE', #377, #8672, #10912 ) ;
#3919 = DIRECTION ( 'NONE',  ( 0.000000000000000000, 0.000000000000000000, 1.000000000000000000 ) ) ;
#3920 = ORIENTED_EDGE ( 'NONE', *, *, #12852, .F. ) ;
#3921 = CARTESIAN_POINT ( 'NONE',  ( 2.789999999999999147, -15.04425356660744839, -20.70663861606288236 ) ) ;
#3922 = DIRECTION ( 'NONE',  ( 0.000000000000000000, 0.000000000000000000, 1.000000000000000000 ) ) ;
#3923 = ORIENTED_EDGE ( 'NONE', *, *, #7892, .F. ) ;
#3924 = ORIENTED_EDGE ( 'NONE', *, *, #14847, .T. ) ;
#3925 = ORIENTED_EDGE ( 'NONE', *, *, #2802, .T. ) ;
#3926 = DIRECTION ( 'NONE',  ( 0.000000000000000000, 0.000000000000000000, 1.000000000000000000 ) ) ;
#3927 = LINE ( 'NONE', #1534, #1906 ) ;
#3928 = EDGE_CURVE ( 'NONE', #1504, #7876, #11846, .T. ) ;
#3929 = EDGE_CURVE ( 'NONE', #5940, #12831, #7790, .T. ) ;
#3930 = LINE ( 'NONE', #8606, #439 ) ;
#3931 = DIRECTION ( 'NONE',  ( 0.000000000000000000, 0.000000000000000000, 1.000000000000000000 ) ) ;
#3932 = CIRCLE ( 'NONE', #9806, 4.000000000000000888 ) ;
#3933 = DIRECTION ( 'NONE',  ( 1.576560579138138762E-17, -1.359337748750801608E-17, 1.000000000000000000 ) ) ;
#3934 = CARTESIAN_POINT ( 'NONE',  ( -0.2000000000000000111, -6.997142273814360713, -0.8000000000000000444 ) ) ;
#3935 = VERTEX_POINT ( 'NONE', #9339 ) ;
#3936 = DIRECTION ( 'NONE',  ( 0.000000000000000000, 0.000000000000000000, 1.000000000000000000 ) ) ;
#3937 = VECTOR ( 'NONE', #9593, 1000.000000000000000 ) ;
#3938 = EDGE_CURVE ( 'NONE', #14803, #9849, #1036, .T. ) ;
#3939 =( NAMED_UNIT ( * ) PLANE_ANGLE_UNIT ( ) SI_UNIT ( $, .RADIAN. ) );
#3940 = ORIENTED_EDGE ( 'NONE', *, *, #46, .F. ) ;
#3941 = EDGE_LOOP ( 'NONE', ( #7656, #7213, #4630, #8940, #7923, #14872, #14071, #4635 ) ) ;
#3942 = DIRECTION ( 'NONE',  ( -1.000000000000000000, -0.000000000000000000, -0.000000000000000000 ) ) ;
#3943 = PLANE ( 'NONE',  #5050 ) ;
#3944 = EDGE_CURVE ( 'NONE', #3945, #1275, #2881, .T. ) ;
#3945 = VERTEX_POINT ( 'NONE', #2421 ) ;
#3946 = UNCERTAINTY_MEASURE_WITH_UNIT (LENGTH_MEASURE( 1.000000000000000082E-05 ), #1883, 'distance_accuracy_value', 'NONE');
#3947 = FACE_OUTER_BOUND ( 'NONE', #9592, .T. ) ;
#3948 = B_SPLINE_CURVE_WITH_KNOTS ( 'NONE', 3,
 ( #6904, #13590, #10291, #985, #9213, #5397, #9068, #9138 ),
 .UNSPECIFIED., .F., .F.,
 ( 4, 2, 2, 4 ),
 ( 4.663089342034314221E-07, 0.001898630032275742084, 0.002847711893946511166, 0.003796793755617280681 ),
 .UNSPECIFIED. ) ;
#3949 = ADVANCED_FACE ( 'NONE', ( #7106 ), #3487, .T. ) ;
#3950 = ORIENTED_EDGE ( 'NONE', *, *, #15174, .T. ) ;
#3951 = CARTESIAN_POINT ( 'NONE',  ( 0.02531912748286561932, 13.68080036884348516, 5.229914364928400339 ) ) ;
#3952 = CARTESIAN_POINT ( 'NONE',  ( 0.02531912748679129854, 11.36963888406687317, 9.232963481057801403 ) ) ;
#3953 = CARTESIAN_POINT ( 'NONE',  ( 1.398397006336996817, -6.091550361990593743, -0.8000000000000000444 ) ) ;
#3954 = CYLINDRICAL_SURFACE ( 'NONE', #14308, 2.524999999999995914 ) ;
#3955 = DIRECTION ( 'NONE',  ( -1.000000000000000000, 0.000000000000000000, -0.000000000000000000 ) ) ;
#3956 = EDGE_LOOP ( 'NONE', ( #12824, #13348, #7937, #2117, #7805 ) ) ;
#3957 = CARTESIAN_POINT ( 'NONE',  ( 0.7795480827049469097, 16.73367785739764813, -5.008579424861385299 ) ) ;
#3958 = SURFACE_SIDE_STYLE ('',( #2069 ) ) ;
#3959 = ORIENTED_EDGE ( 'NONE', *, *, #1269, .T. ) ;
#3960 = ORIENTED_EDGE ( 'NONE', *, *, #4941, .F. ) ;
#3961 = LINE ( 'NONE', #13171, #1671 ) ;
#3962 = CYLINDRICAL_SURFACE ( 'NONE', #8060, 2.524999999999995914 ) ;
#3963 = CARTESIAN_POINT ( 'NONE',  ( 0.07181525696555239591, 24.78695292654921545, 5.344212458769448837 ) ) ;
#3964 = DIRECTION ( 'NONE',  ( -0.000000000000000000, -0.000000000000000000, 1.000000000000000000 ) ) ;
#3965 = B_SPLINE_CURVE_WITH_KNOTS ( 'NONE', 3,
 ( #7921, #6691, #771, #13683 ),
 .UNSPECIFIED., .F., .F.,
 ( 4, 4 ),
 ( 2.135345996173300665E-07, 0.0006888010880210822381 ),
 .UNSPECIFIED. ) ;
#3966 = VERTEX_POINT ( 'NONE', #8176 ) ;
#3967 = FACE_OUTER_BOUND ( 'NONE', #5270, .T. ) ;
#3968 = DIRECTION ( 'NONE',  ( 0.000000000000000000, 0.000000000000000000, 1.000000000000000000 ) ) ;
#3969 = CYLINDRICAL_SURFACE ( 'NONE', #12493, 3.799999999999998934 ) ;
#3970 = SURFACE_SIDE_STYLE ('',( #5059 ) ) ;
#3971 = ORIENTED_EDGE ( 'NONE', *, *, #5646, .F. ) ;
#3972 = ORIENTED_EDGE ( 'NONE', *, *, #13956, .T. ) ;
#3973 = ORIENTED_EDGE ( 'NONE', *, *, #13888, .T. ) ;
#3974 = CARTESIAN_POINT ( 'NONE',  ( 1.039999999999997149, -24.89775460606822577, -12.96210679857813730 ) ) ;
#3975 = CARTESIAN_POINT ( 'NONE',  ( -5.209999999999999964, 0.000000000000000000, 0.000000000000000000 ) ) ;
#3976 = ADVANCED_FACE ( 'NONE', ( #5732 ), #14095, .F. ) ;
#3977 = DIRECTION ( 'NONE',  ( 0.000000000000000000, 0.000000000000000000, 1.000000000000000000 ) ) ;
#3978 = CARTESIAN_POINT ( 'NONE',  ( 1.394999999999998685, 24.89775460606851354, -12.96210679857759374 ) ) ;
#3979 = DIRECTION ( 'NONE',  ( 1.000000000000000000, 0.000000000000000000, 0.000000000000000000 ) ) ;
#3980 = CARTESIAN_POINT ( 'NONE',  ( 18.71314632718394222, -23.25585687728512241, -2.000000000000000000 ) ) ;
#3981 = DIRECTION ( 'NONE',  ( 0.000000000000000000, -1.000000000000000000, 0.000000000000000000 ) ) ;
#3982 = LINE ( 'NONE', #507, #5759 ) ;
#3983 = ORIENTED_EDGE ( 'NONE', *, *, #3602, .T. ) ;
#3984 = DIRECTION ( 'NONE',  ( -0.000000000000000000, -0.000000000000000000, -1.000000000000000000 ) ) ;
#3985 = AXIS2_PLACEMENT_3D ( 'NONE', #11351, #10129, #4517 ) ;
#3986 = DIRECTION ( 'NONE',  ( -1.000000000000000000, 0.000000000000000000, 0.000000000000000000 ) ) ;
#3987 = CARTESIAN_POINT ( 'NONE',  ( 2.724444381390116021, -21.84113606038314259, 12.72236714503155142 ) ) ;
#3988 = EDGE_CURVE ( 'NONE', #8704, #1423, #14168, .T. ) ;
#3989 = VERTEX_POINT ( 'NONE', #12851 ) ;
#3990 = ADVANCED_FACE ( 'NONE', ( #10567 ), #3642, .F. ) ;
#3991 = CARTESIAN_POINT ( 'NONE',  ( 2.582362745529149795, -10.30022894898814734, 12.04200105039466528 ) ) ;
#3992 = CARTESIAN_POINT ( 'NONE',  ( 0.2076373213219109837, -15.57879356040265151, 2.899259574942692819 ) ) ;
#3993 = VERTEX_POINT ( 'NONE', #8329 ) ;
#3994 = ORIENTED_EDGE ( 'NONE', *, *, #6958, .T. ) ;
#3995 = CARTESIAN_POINT ( 'NONE',  ( 2.783068888626320625, -9.685942809246897767, -22.53293026234513619 ) ) ;
#3996 = CARTESIAN_POINT ( 'NONE',  ( 111.6227766016837961, 7.610970684806392799E-15, 6.000000000000000000 ) ) ;
#3997 = AXIS2_PLACEMENT_3D ( 'NONE', #8507, #13198, #429 ) ;
#3998 = DIRECTION ( 'NONE',  ( 0.4571871344001385284, 0.8893705212896308998, -0.000000000000000000 ) ) ;
#3999 = FACE_OUTER_BOUND ( 'NONE', #2990, .T. ) ;
#4000 = DIRECTION ( 'NONE',  ( -1.000000000000000000, 0.000000000000000000, -0.000000000000000000 ) ) ;
#4001 = B_SPLINE_CURVE_WITH_KNOTS ( 'NONE', 3,
 ( #10442, #15060, #2147, #6834, #6908, #10214, #4533, #5618 ),
 .UNSPECIFIED., .F., .F.,
 ( 4, 2, 2, 4 ),
 ( 2.154797737799112159E-07, 0.001895231411415137677, 0.002842739377235818047, 0.003790247343056497766 ),
 .UNSPECIFIED. ) ;
#4002 = ORIENTED_EDGE ( 'NONE', *, *, #2531, .F. ) ;
#4003 = CARTESIAN_POINT ( 'NONE',  ( -16.14082873121598993, -7.414910804916202913, -3.000000000000000000 ) ) ;
#4004 = EDGE_CURVE ( 'NONE', #851, #12497, #9560, .T. ) ;
#4005 =( NAMED_UNIT ( * ) PLANE_ANGLE_UNIT ( ) SI_UNIT ( $, .RADIAN. ) );
#4006 = VERTEX_POINT ( 'NONE', #11704 ) ;
#4007 = ORIENTED_EDGE ( 'NONE', *, *, #14651, .F. ) ;
#4008 = VERTEX_POINT ( 'NONE', #10714 ) ;
#4009 = CARTESIAN_POINT ( 'NONE',  ( 2.789999999999999147, -2.336989772644440855, 24.63872515616082026 ) ) ;
#4010 = CARTESIAN_POINT ( 'NONE',  ( 0.000000000000000000, -1.948757464274271767, 13.87420763704360915 ) ) ;
#4011 = ORIENTED_EDGE ( 'NONE', *, *, #11252, .F. ) ;
#4012 = EDGE_CURVE ( 'NONE', #3271, #497, #7178, .T. ) ;
#4013 = CARTESIAN_POINT ( 'NONE',  ( 32.66827876307085887, -1.833751565556681173, 2.999999999999999112 ) ) ;
#4014 = ADVANCED_FACE ( 'NONE', ( #19 ), #4890, .F. ) ;
#4015 = ORIENTED_EDGE ( 'NONE', *, *, #10395, .T. ) ;
#4016 = B_SPLINE_CURVE_WITH_KNOTS ( 'NONE', 3,
 ( #559, #10870, #5280, #8568, #3963, #14727 ),
 .UNSPECIFIED., .F., .F.,
 ( 4, 2, 4 ),
 ( 4.462636677693390501E-07, 0.001879885020955133004, 0.003759323778242496666 ),
 .UNSPECIFIED. ) ;
#4017 = DIRECTION ( 'NONE',  ( 1.000000000000000000, -0.000000000000000000, -0.000000000000000000 ) ) ;
#4018 = CARTESIAN_POINT ( 'NONE',  ( 2.783069004973550253, -23.92277630352791107, -5.408431875071696204 ) ) ;
#4019 = EDGE_CURVE ( 'NONE', #3700, #10457, #3020, .T. ) ;
#4020 = ADVANCED_FACE ( 'NONE', ( #10493 ), #15108, .T. ) ;
#4021 = PRODUCT_DEFINITION_FORMATION_WITH_SPECIFIED_SOURCE ( 'ANY', '', #10699, .NOT_KNOWN. ) ;
#4022 = FACE_OUTER_BOUND ( 'NONE', #8399, .T. ) ;
#4023 = B_SPLINE_CURVE_WITH_KNOTS ( 'NONE', 3,
 ( #9012, #14860, #4018, #5492 ),
 .UNSPECIFIED., .F., .F.,
 ( 4, 4 ),
 ( 0.005258214619651960589, 0.005948481662034167325 ),
 .UNSPECIFIED. ) ;
#4024 = CARTESIAN_POINT ( 'NONE',  ( -20.63749999999999929, 0.000000000000000000, 0.000000000000000000 ) ) ;
#4025 = CARTESIAN_POINT ( 'NONE',  ( 0.2076372544708505186, 12.04200105039484825, -10.30022894898793595 ) ) ;
#4026 = ORIENTED_EDGE ( 'NONE', *, *, #8740, .F. ) ;
#4027 = DIRECTION ( 'NONE',  ( 0.9995917534020515305, -0.02857142857142857054, 0.000000000000000000 ) ) ;
#4028 = CARTESIAN_POINT ( 'NONE',  ( 0.006931069955679173590, 18.43696893154758598, 16.17493693894884998 ) ) ;
#4029 = VECTOR ( 'NONE', #8322, 1000.000000000000000 ) ;
#4030 = ORIENTED_EDGE ( 'NONE', *, *, #3737, .T. ) ;
#4031 = EDGE_LOOP ( 'NONE', ( #4170, #1831, #14644, #4515 ) ) ;
#4032 = DIRECTION ( 'NONE',  ( 1.000000000000000000, -0.000000000000000000, -0.000000000000000000 ) ) ;
#4033 = FACE_BOUND ( 'NONE', #15004, .T. ) ;
#4034 = CARTESIAN_POINT ( 'NONE',  ( 2.718131847775118182, 24.78765742476139522, 5.344160105508784397 ) ) ;
#4035 = EDGE_CURVE ( 'NONE', #7956, #10751, #12821, .T. ) ;
#4036 = AXIS2_PLACEMENT_3D ( 'NONE', #1469, #7080, #10612 ) ;
#4037 = ADVANCED_FACE ( 'NONE', ( #12929 ), #11629, .F. ) ;
#4038 = CIRCLE ( 'NONE', #12848, 2.524999999999998579 ) ;
#4039 = DIRECTION ( 'NONE',  ( 1.000000000000000000, 0.000000000000000000, 0.000000000000000000 ) ) ;
#4040 = AXIS2_PLACEMENT_3D ( 'NONE', #3785, #8763, #2646 ) ;
#4042 = VERTEX_POINT ( 'NONE', #1721 ) ;
#4041 = EDGE_CURVE ( 'NONE', #5949, #4081, #550, .T. ) ;
#4043 = DIRECTION ( 'NONE',  ( 0.000000000000000000, 0.000000000000000000, 1.000000000000000000 ) ) ;
#4044 = DIRECTION ( 'NONE',  ( 0.000000000000000000, 0.000000000000000000, 1.000000000000000000 ) ) ;
#4045 = CARTESIAN_POINT ( 'NONE',  ( 0.02436607992775978102, 16.37294372382885044, -18.55949924794875017 ) ) ;
#4046 = DIRECTION ( 'NONE',  ( 0.000000000000000000, 0.000000000000000000, 1.000000000000000000 ) ) ;
#4047 = ORIENTED_EDGE ( 'NONE', *, *, #9107, .T. ) ;
#4048 = ORIENTED_EDGE ( 'NONE', *, *, #13312, .T. ) ;
#4049 = CIRCLE ( 'NONE', #7971, 3.000000000000000888 ) ;
#4050 = CIRCLE ( 'NONE', #1845, 4.599999999999999645 ) ;
#4051 = EDGE_CURVE ( 'NONE', #14255, #14793, #301, .T. ) ;
#4052 = ORIENTED_EDGE ( 'NONE', *, *, #170, .T. ) ;
#4053 = CARTESIAN_POINT ( 'NONE',  ( 1.749999999999998002, 4.147968289691672084, -27.76164181293047406 ) ) ;
#4054 = CYLINDRICAL_SURFACE ( 'NONE', #6084, 3.000000000000000888 ) ;
#4055 = CARTESIAN_POINT ( 'NONE',  ( 13.28797974610715116, -21.11867004231547540, 7.000000000000000000 ) ) ;
#4056 = DIRECTION ( 'NONE',  ( 0.000000000000000000, 0.000000000000000000, 1.000000000000000000 ) ) ;
#4057 = PRODUCT_CONTEXT ( 'NONE', #14709, 'mechanical' ) ;
#4058 = LINE ( 'NONE', #5071, #14048 ) ;
#4059 = DIRECTION ( 'NONE',  ( -1.000000000000000000, 0.000000000000000000, 0.000000000000000000 ) ) ;
#4060 = DIRECTION ( 'NONE',  ( 0.000000000000000000, 0.000000000000000000, 1.000000000000000000 ) ) ;
#4061 = AXIS2_PLACEMENT_3D ( 'NONE', #11789, #14262, #3724 ) ;
#4062 = ORIENTED_EDGE ( 'NONE', *, *, #399, .T. ) ;
#4063 = DIRECTION ( 'NONE',  ( -0.4571871344001416926, -0.8893705212896291235, -0.000000000000000000 ) ) ;
#4064 = DIRECTION ( 'NONE',  ( 0.000000000000000000, 0.000000000000000000, 1.000000000000000000 ) ) ;
#4065 = CIRCLE ( 'NONE', #2331, 17.95481323787947758 ) ;
#4066 = DIRECTION ( 'NONE',  ( -1.000000000000000000, -0.000000000000000000, -0.000000000000000000 ) ) ;
#4067 = EDGE_LOOP ( 'NONE', ( #13062, #11992, #7774, #1629 ) ) ;
#4068 = DIRECTION ( 'NONE',  ( -0.000000000000000000, -0.000000000000000000, 1.000000000000000000 ) ) ;
#4069 = FACE_OUTER_BOUND ( 'NONE', #11581, .T. ) ;
#4070 = ORIENTED_EDGE ( 'NONE', *, *, #2107, .F. ) ;
#4071 = ORIENTED_EDGE ( 'NONE', *, *, #13327, .F. ) ;
#4072 = CARTESIAN_POINT ( 'NONE',  ( 2.789999999999999147, -24.34211360614294506, -7.909232158575071558 ) ) ;
#4073 = VECTOR ( 'NONE', #7837, 1000.000000000000000 ) ;
#4074 = CARTESIAN_POINT ( 'NONE',  ( 2.789999999999999147, -22.71065055754459650, 9.836394144775621129 ) ) ;
#4075 = CIRCLE ( 'NONE', #6272, 3.000000000000002665 ) ;
#4076 = CARTESIAN_POINT ( 'NONE',  ( 1.749999999999998002, -12.96210679857767367, -24.89775460606847091 ) ) ;
#4077 = CARTESIAN_POINT ( 'NONE',  ( 2.782650468023970092, 2.217353748341931663, 14.24968354755769440 ) ) ;
#4078 = DIRECTION ( 'NONE',  ( -1.576560579138138762E-17, 1.359337748750801608E-17, -1.000000000000000000 ) ) ;
#4079 = FACE_OUTER_BOUND ( 'NONE', #8975, .T. ) ;
#4080 = ADVANCED_FACE ( 'NONE', ( #10931 ), #2789, .T. ) ;
#4081 = VERTEX_POINT ( 'NONE', #6107 ) ;
#4082 = B_SPLINE_CURVE_WITH_KNOTS ( 'NONE', 3,
 ( #4966, #1730, #9720, #9639 ),
 .UNSPECIFIED., .F., .F.,
 ( 4, 4 ),
 ( 3.059063720746937335E-07, 0.0006888942284914199117 ),
 .UNSPECIFIED. ) ;
#4083 = CARTESIAN_POINT ( 'NONE',  ( 0.3363705501000964215, -6.891763197764913862, 6.000000000000000000 ) ) ;
#4084 = CIRCLE ( 'NONE', #891, 4.000000000000000000 ) ;
#4085 = CARTESIAN_POINT ( 'NONE',  ( 2.765633920072235963, 24.63872515616082737, 2.336989772644355146 ) ) ;
#4086 = ORIENTED_EDGE ( 'NONE', *, *, #13541, .T. ) ;
#4087 = ORIENTED_EDGE ( 'NONE', *, *, #2915, .T. ) ;
#4088 = ORIENTED_EDGE ( 'NONE', *, *, #13114, .T. ) ;
#4089 = CARTESIAN_POINT ( 'NONE',  ( 2.789999999999999147, 23.17675759782041212, -7.772527002114516748 ) ) ;
#4090 = DIRECTION ( 'NONE',  ( 0.9728364810787193395, 0.2314933715733012709, 0.000000000000000000 ) ) ;
#4091 = AXIS2_PLACEMENT_3D ( 'NONE', #5161, #360, #3916 ) ;
#4092 = ORIENTED_EDGE ( 'NONE', *, *, #12642, .F. ) ;
#4093 = AXIS2_PLACEMENT_3D ( 'NONE', #12482, #6644, #10024 ) ;
#4094 = UNCERTAINTY_MEASURE_WITH_UNIT (LENGTH_MEASURE( 1.000000000000000082E-05 ), #10539, 'distance_accuracy_value', 'NONE');
#4095 = MECHANICAL_DESIGN_GEOMETRIC_PRESENTATION_REPRESENTATION (  '', ( #10716 ), #14895 ) ;
#4096 = DIRECTION ( 'NONE',  ( 0.000000000000000000, 0.000000000000000000, 1.000000000000000000 ) ) ;
#4097 = VECTOR ( 'NONE', #7107, 1000.000000000000000 ) ;
#4098 = CARTESIAN_POINT ( 'NONE',  ( 50.00050000000000239, 0.000000000000000000, 0.000000000000000000 ) ) ;
#4099 = VERTEX_POINT ( 'NONE', #13391 ) ;
#4100 = CARTESIAN_POINT ( 'NONE',  ( -14.40394475573011945, -10.79473832354794460, -3.794707603699265519E-15 ) ) ;
#4101 = DIRECTION ( 'NONE',  ( 0.000000000000000000, 0.000000000000000000, 1.000000000000000000 ) ) ;
#4102 = CARTESIAN_POINT ( 'NONE',  ( 62.65957446808508280, 26.91300136313512681, 4.000000000000000000 ) ) ;
#4103 = EDGE_CURVE ( 'NONE', #9731, #8563, #14324, .T. ) ;
#4104 = CYLINDRICAL_SURFACE ( 'NONE', #12084, 2.524999999999999023 ) ;
#4105 = DIRECTION ( 'NONE',  ( -1.000000000000000000, -0.000000000000000000, -0.000000000000000000 ) ) ;
#4106 = CIRCLE ( 'NONE', #5353, 17.95481323787947758 ) ;
#4107 = EDGE_LOOP ( 'NONE', ( #1038, #1645, #1867, #4644 ) ) ;
#4108 = AXIS2_PLACEMENT_3D ( 'NONE', #3378, #13754, #11586 ) ;
#4109 = CARTESIAN_POINT ( 'NONE',  ( 0.4522159317772137532, 15.84984805378638484, -5.191253194755847566 ) ) ;
#4110 = CARTESIAN_POINT ( 'NONE',  ( -1.398397006336996817, -6.091550361990593743, -0.8000000000000000444 ) ) ;
#4111 = TOROIDAL_SURFACE ( 'NONE', #13428, 14.01039946648073986, 8.000000000000000000 ) ;
#4112 = ORIENTED_EDGE ( 'NONE', *, *, #14328, .T. ) ;
#4113 = VERTEX_POINT ( 'NONE', #1642 ) ;
#4114 = DIRECTION ( 'NONE',  ( 1.000000000000000000, 0.000000000000000000, 0.000000000000000000 ) ) ;
#4115 = CARTESIAN_POINT ( 'NONE',  ( 0.000000000000000000, 0.000000000000000000, 5.500000000000000000 ) ) ;
#4116 = PRODUCT_RELATED_PRODUCT_CATEGORY ( 'part', '', ( #11166 ) ) ;
#4117 = EDGE_CURVE ( 'NONE', #6654, #2553, #10578, .T. ) ;
#4118 = EDGE_CURVE ( 'NONE', #6030, #8726, #1416, .T. ) ;
#4119 = CARTESIAN_POINT ( 'NONE',  ( 2.765633920072236851, 24.15498966839963302, 5.391175441198700291 ) ) ;
#4120 = VECTOR ( 'NONE', #2044, 1000.000000000000000 ) ;
#4121 = DIRECTION ( 'NONE',  ( 0.000000000000000000, 0.000000000000000000, 1.000000000000000000 ) ) ;
#4122 = VECTOR ( 'NONE', #13651, 1000.000000000000000 ) ;
#4123 = ORIENTED_EDGE ( 'NONE', *, *, #10600, .F. ) ;
#4124 = FACE_OUTER_BOUND ( 'NONE', #1478, .T. ) ;
#4125 = CARTESIAN_POINT ( 'NONE',  ( 0.02436607992776325046, 16.37294372382858398, 18.55949924794898465 ) ) ;
#4126 = AXIS2_PLACEMENT_3D ( 'NONE', #9819, #13504, #14514 ) ;
#4127 = VECTOR ( 'NONE', #3022, 1000.000000000000000 ) ;
#4128 = ORIENTED_EDGE ( 'NONE', *, *, #12202, .F. ) ;
#4129 = CARTESIAN_POINT ( 'NONE',  ( -12.16787677823033142, -7.794738323547949932, 14.99999999999999822 ) ) ;
#4130 = VERTEX_POINT ( 'NONE', #9861 ) ;
#4131 = ADVANCED_FACE ( 'NONE', ( #12079 ), #5120, .T. ) ;
#4132 = VERTEX_POINT ( 'NONE', #14637 ) ;
#4133 = EDGE_CURVE ( 'NONE', #7876, #2548, #8903, .T. ) ;
#4134 = ORIENTED_EDGE ( 'NONE', *, *, #9472, .F. ) ;
#4135 = AXIS2_PLACEMENT_3D ( 'NONE', #13484, #2958, #7646 ) ;
#4136 = CARTESIAN_POINT ( 'NONE',  ( -20.63749999999999574, 7.347880794884121708E-16, 6.000000000000001776 ) ) ;
#4137 = FACE_OUTER_BOUND ( 'NONE', #6773, .T. ) ;
#4138 = ADVANCED_FACE ( 'NONE', ( #6330 ), #3954, .F. ) ;
#4139 = AXIS2_PLACEMENT_3D ( 'NONE', #1754, #359, #8660 ) ;
#4140 = DIRECTION ( 'NONE',  ( 1.000000000000000000, 0.000000000000000000, 0.000000000000000000 ) ) ;
#4141 = AXIS2_PLACEMENT_3D ( 'NONE', #10799, #12166, #9803 ) ;
#4142 = DIRECTION ( 'NONE',  ( 1.000000000000000000, 0.000000000000000000, 0.000000000000000000 ) ) ;
#4143 = CARTESIAN_POINT ( 'NONE',  ( 2.789999999999999147, 1.621424371464993087E-13, -15.47981323787947794 ) ) ;
#4144 = DIRECTION ( 'NONE',  ( 1.576560579138138762E-17, -1.359337748750801608E-17, 1.000000000000000000 ) ) ;
#4145 = DIRECTION ( 'NONE',  ( -1.000000000000000000, -0.000000000000000000, -0.000000000000000000 ) ) ;
#4146 = ADVANCED_FACE ( 'NONE', ( #13314 ), #7488, .T. ) ;
#4147 = ORIENTED_EDGE ( 'NONE', *, *, #14712, .F. ) ;
#4148 = CARTESIAN_POINT ( 'NONE',  ( 0.000000000000000000, 0.000000000000000000, 3.895000000000000462 ) ) ;
#4149 = CARTESIAN_POINT ( 'NONE',  ( 2.783068945535914995, 2.248820353272968919, 24.42321038836783131 ) ) ;
#4150 = CARTESIAN_POINT ( 'NONE',  ( 0.000000000000000000, -1.991882183130475603, 24.04302995059966719 ) ) ;
#4151 = ORIENTED_EDGE ( 'NONE', *, *, #10975, .T. ) ;
#4152 = CIRCLE ( 'NONE', #669, 2.524999999999999467 ) ;
#4153 = CARTESIAN_POINT ( 'NONE',  ( 2.789999999999999147, 2.680914349914567470E-13, -23.06981291497571362 ) ) ;
#4154 = DIRECTION ( 'NONE',  ( 0.000000000000000000, 0.000000000000000000, 1.000000000000000000 ) ) ;
#4155 = VERTEX_POINT ( 'NONE', #7564 ) ;
#4156 = EDGE_LOOP ( 'NONE', ( #9583, #3189, #2671, #11607, #13630, #1422 ) ) ;
#4157 = CARTESIAN_POINT ( 'NONE',  ( 2.141980652367355464, -6.189445006155633422, -0.8000000000000000444 ) ) ;
#4158 = LINE ( 'NONE', #4074, #15170 ) ;
#4159 = CARTESIAN_POINT ( 'NONE',  ( 2.601776096565022289, -12.84621645676828372, -22.54313264455027976 ) ) ;
#4160 = DIRECTION ( 'NONE',  ( 0.000000000000000000, 0.000000000000000000, 1.000000000000000000 ) ) ;
#4161 = DIRECTION ( 'NONE',  ( -1.000000000000000000, 0.000000000000000000, 0.000000000000000000 ) ) ;
#4162 = CARTESIAN_POINT ( 'NONE',  ( 0.02436607992775761261, 22.71065055754452544, 9.836394144775786330 ) ) ;
#4163 = AXIS2_PLACEMENT_3D ( 'NONE', #8340, #8777, #9573 ) ;
#4164 = ORIENTED_EDGE ( 'NONE', *, *, #1444, .T. ) ;
#4165 = B_SPLINE_CURVE_WITH_KNOTS ( 'NONE', 3,
 ( #10595, #10364, #4838, #12810 ),
 .UNSPECIFIED., .F., .F.,
 ( 4, 4 ),
 ( 0.0006045424356927869836, 0.0006887909409525213005 ),
 .UNSPECIFIED. ) ;
#4166 = CARTESIAN_POINT ( 'NONE',  ( -6.154400080602563004E-14, -11.12234047011196658, 8.842064619038488615 ) ) ;
#4167 = CARTESIAN_POINT ( 'NONE',  ( 0.000000000000000000, 7.909232158574813099, 24.34211360614303388 ) ) ;
#4168 = ORIENTED_EDGE ( 'NONE', *, *, #11858, .T. ) ;
#4169 =( LENGTH_UNIT ( ) NAMED_UNIT ( * ) SI_UNIT ( .MILLI., .METRE. ) );
#4170 = ORIENTED_EDGE ( 'NONE', *, *, #6461, .T. ) ;
#4171 = ORIENTED_EDGE ( 'NONE', *, *, #1457, .F. ) ;
#4172 = SHAPE_REPRESENTATION ( 'short pitch roller chain wheel_s_iso_Chain wheel ISO - 12Z 05B-1 --12SA8.0N', ( #1376 ), #13900 ) ;
#4173 = ORIENTED_EDGE ( 'NONE', *, *, #9950, .F. ) ;
#4174 = AXIS2_PLACEMENT_3D ( 'NONE', #11438, #7846, #12528 ) ;
#4175 = CARTESIAN_POINT ( 'NONE',  ( 0.007327564474061089815, 9.044896821682200994, 11.23174270417332465 ) ) ;
#4176 = DIRECTION ( 'NONE',  ( 0.2314933715733012709, -0.9728364810787193395, 0.000000000000000000 ) ) ;
#4177 = EDGE_CURVE ( 'NONE', #212, #1071, #9392, .T. ) ;
#4178 = DIRECTION ( 'NONE',  ( -1.000000000000000000, 0.000000000000000000, 0.000000000000000000 ) ) ;
#4179 = DIRECTION ( 'NONE',  ( 1.000000000000000000, 0.000000000000000000, 0.000000000000000000 ) ) ;
#4180 = EDGE_LOOP ( 'NONE', ( #7200, #2987, #11360, #3326, #10873, #2419, #4855, #7458, #3718, #3091 ) ) ;
#4181 = DIRECTION ( 'NONE',  ( -0.5416238976136773520, 0.8406209333187990573, 0.000000000000000000 ) ) ;
#4182 = FACE_OUTER_BOUND ( 'NONE', #13765, .T. ) ;
#4183 = CIRCLE ( 'NONE', #6382, 2.524999999999999467 ) ;
#4184 = DIRECTION ( 'NONE',  ( 1.576560579138138762E-17, -1.359337748750801608E-17, 1.000000000000000000 ) ) ;
#4185 = CARTESIAN_POINT ( 'NONE',  ( 0.07181525068722517668, 2.576941577947404305, 25.22524549359951251 ) ) ;
#4186 = ADVANCED_FACE ( 'NONE', ( #11089 ), #4104, .F. ) ;
#4187 = ORIENTED_EDGE ( 'NONE', *, *, #8071, .F. ) ;
#4188 = CARTESIAN_POINT ( 'NONE',  ( 0.1085714285714285687, -3.798448662927795372, 0.000000000000000000 ) ) ;
#4189 = EDGE_CURVE ( 'NONE', #7258, #13917, #8471, .T. ) ;
#4190 = CARTESIAN_POINT ( 'NONE',  ( 1.749999999999999778, -12.83329210556822453, -12.55714665600001290 ) ) ;
#4191 = B_SPLINE_CURVE_WITH_KNOTS ( 'NONE', 3,
 ( #8826, #10900, #13439, #3836, #2693, #6146, #365, #13212 ),
 .UNSPECIFIED., .F., .F.,
 ( 4, 2, 2, 4 ),
 ( 4.663089536341708793E-07, 0.001898630414085407348, 0.002847712466651294069, 0.003796794519217180572 ),
 .UNSPECIFIED. ) ;
#4192 = ORIENTED_EDGE ( 'NONE', *, *, #15179, .F. ) ;
#4193 = ORIENTED_EDGE ( 'NONE', *, *, #9625, .F. ) ;
#4194 = FACE_OUTER_BOUND ( 'NONE', #3414, .T. ) ;
#4195 = EDGE_CURVE ( 'NONE', #13780, #4420, #8913, .T. ) ;
#4196 = CARTESIAN_POINT ( 'NONE',  ( 0.07186811453410638095, -16.91241718342012490, 18.89333555428548905 ) ) ;
#4197 = VERTEX_POINT ( 'NONE', #10247 ) ;
#4198 = DIRECTION ( 'NONE',  ( 0.000000000000000000, 0.000000000000000000, 1.000000000000000000 ) ) ;
#4199 = EDGE_LOOP ( 'NONE', ( #6425, #13995, #11553, #3879 ) ) ;
#4200 = DIRECTION ( 'NONE',  ( -0.000000000000000000, -1.000000000000000000, -0.000000000000000000 ) ) ;
#4201 = DIRECTION ( 'NONE',  ( 0.000000000000000000, 0.000000000000000000, 1.000000000000000000 ) ) ;
#4202 = ORIENTED_EDGE ( 'NONE', *, *, #11610, .F. ) ;
#4203 = DIRECTION ( 'NONE',  ( 1.000000000000000000, 0.000000000000000000, 0.000000000000000000 ) ) ;
#4204 = EDGE_CURVE ( 'NONE', #13954, #6351, #5721, .T. ) ;
#4205 = EDGE_CURVE ( 'NONE', #11809, #11548, #14421, .T. ) ;
#4206 = CARTESIAN_POINT ( 'NONE',  ( 1.149999999999998135, 0.000000000000000000, 0.000000000000000000 ) ) ;
#4207 = ORIENTED_EDGE ( 'NONE', *, *, #13839, .T. ) ;
#4208 = ORIENTED_EDGE ( 'NONE', *, *, #7877, .T. ) ;
#4209 = ORIENTED_EDGE ( 'NONE', *, *, #10286, .T. ) ;
#4210 = LINE ( 'NONE', #7736, #4612 ) ;
#4211 = CARTESIAN_POINT ( 'NONE',  ( 2.646101151984011857, -14.59528211758545524, 5.279841123860813390 ) ) ;
#4212 = CARTESIAN_POINT ( 'NONE',  ( 0.006974663525959075641, 12.53640742967783694, -21.08118142846890208 ) ) ;
#4213 = CARTESIAN_POINT ( 'NONE',  ( 0.1717365941144614327, -6.008326913195983998, 0.000000000000000000 ) ) ;
#4214 = CARTESIAN_POINT ( 'NONE',  ( 79.18363542992865689, -10.13606076167855541, 4.000000000000003553 ) ) ;
#4215 = DIRECTION ( 'NONE',  ( 1.000000000000000000, 0.000000000000000000, 0.000000000000000000 ) ) ;
#4216 = DIRECTION ( 'NONE',  ( 0.000000000000000000, 0.000000000000000000, 1.000000000000000000 ) ) ;
#4217 = EDGE_CURVE ( 'NONE', #5125, #134, #5351, .T. ) ;
#4218 = ORIENTED_EDGE ( 'NONE', *, *, #6938, .F. ) ;
#4219 = DIRECTION ( 'NONE',  ( 0.000000000000000000, 0.000000000000000000, 1.000000000000000000 ) ) ;
#4220 = DIRECTION ( 'NONE',  ( -1.000000000000000000, 0.000000000000000000, 0.000000000000000000 ) ) ;
#4221 = CARTESIAN_POINT ( 'NONE',  ( 0.000000000000000000, 0.000000000000000000, 7.000000000000000000 ) ) ;
#4222 = EDGE_CURVE ( 'NONE', #10087, #8808, #11565, .T. ) ;
#4223 = EDGE_CURVE ( 'NONE', #13724, #5313, #11243, .T. ) ;
#4224 = VERTEX_POINT ( 'NONE', #5424 ) ;
#4225 = DIRECTION ( 'NONE',  ( -1.000000000000000000, -0.000000000000000000, -0.000000000000000000 ) ) ;
#4226 = CYLINDRICAL_SURFACE ( 'NONE', #3341, 13.19999999999999929 ) ;
#4227 = ORIENTED_EDGE ( 'NONE', *, *, #3412, .T. ) ;
#4228 = VERTEX_POINT ( 'NONE', #7637 ) ;
#4229 = CYLINDRICAL_SURFACE ( 'NONE', #14667, 3.000000000000002665 ) ;
#4230 = CARTESIAN_POINT ( 'NONE',  ( 0.02531912748679520167, -11.36963888406680923, -9.232963481057881339 ) ) ;
#4231 = CARTESIAN_POINT ( 'NONE',  ( 1.039999999999999147, -17.39253030560838198, -4.458161950358684678 ) ) ;
#4232 = CARTESIAN_POINT ( 'NONE',  ( 67.23404255319145761, 28.93147646537025963, 4.000000000000000000 ) ) ;
#4233 = CARTESIAN_POINT ( 'NONE',  ( 2.789999999999999147, 14.59528211760002137, 5.279841123860918195 ) ) ;
#4234 = CIRCLE ( 'NONE', #11590, 24.12539914357697768 ) ;
#4235 = CARTESIAN_POINT ( 'NONE',  ( 0.7592463834391182109, 24.80264696524898937, -12.05220173035413112 ) ) ;
#4236 = CARTESIAN_POINT ( 'NONE',  ( -19.40394475573012301, -13.79473832354794993, 16.99999999999999645 ) ) ;
#4237 = ORIENTED_EDGE ( 'NONE', *, *, #14468, .T. ) ;
#4238 = CARTESIAN_POINT ( 'NONE',  ( -15.94493884710238696, -7.321218896460230496, -3.000000000000000000 ) ) ;
#4239 = DIRECTION ( 'NONE',  ( -1.000000000000000000, 0.000000000000000000, -0.000000000000000000 ) ) ;
#4240 = EDGE_CURVE ( 'NONE', #11326, #7126, #1872, .T. ) ;
#4241 = ORIENTED_EDGE ( 'NONE', *, *, #4788, .F. ) ;
#4242 = SURFACE_STYLE_USAGE ( .BOTH. , #12753 ) ;
#4243 = TOROIDAL_SURFACE ( 'NONE', #5238, 4.100000000000000533, 0.1000000000000001582 ) ;
#4244 = CIRCLE ( 'NONE', #5714, 2.524999999999995914 ) ;
#4245 = ORIENTED_EDGE ( 'NONE', *, *, #2287, .T. ) ;
#4246 = ORIENTED_EDGE ( 'NONE', *, *, #4012, .T. ) ;
#4247 = ORIENTED_EDGE ( 'NONE', *, *, #9002, .T. ) ;
#4248 = DIRECTION ( 'NONE',  ( 1.000000000000000000, -0.000000000000000000, -0.000000000000000000 ) ) ;
#4249 = DIRECTION ( 'NONE',  ( -1.000000000000000000, -0.000000000000000000, -0.000000000000000000 ) ) ;
#4250 = EDGE_CURVE ( 'NONE', #10187, #552, #11385, .T. ) ;
#4251 = CARTESIAN_POINT ( 'NONE',  ( 0.007349531976028004371, -14.24968354755767130, -2.217353748342081321 ) ) ;
#4252 = DIRECTION ( 'NONE',  ( 0.000000000000000000, 0.000000000000000000, 1.000000000000000000 ) ) ;
#4253 = ORIENTED_EDGE ( 'NONE', *, *, #9574, .T. ) ;
#4254 = LINE ( 'NONE', #12075, #2815 ) ;
#4255 = DIRECTION ( 'NONE',  ( 1.000000000000000000, 1.734723475976807341E-16, 2.081668171172168908E-15 ) ) ;
#4256 = CARTESIAN_POINT ( 'NONE',  ( 0.7589665089996477931, -12.05173163741739906, 24.80232951178374279 ) ) ;
#4257 = CARTESIAN_POINT ( 'NONE',  ( 0.4386599019957485579, -23.41653927703718097, 12.93238701107298283 ) ) ;
#4258 = ADVANCED_FACE ( 'NONE', ( #11161 ), #7709, .T. ) ;
#4259 = ORIENTED_EDGE ( 'NONE', *, *, #6450, .T. ) ;
#4260 = DIRECTION ( 'NONE',  ( 0.000000000000000000, 0.000000000000000000, 1.000000000000000000 ) ) ;
#4261 = CARTESIAN_POINT ( 'NONE',  ( 4.872650870659752442, 0.4273491293402468805, -0.8000000000000000444 ) ) ;
#4262 = ORIENTED_EDGE ( 'NONE', *, *, #3631, .F. ) ;
#4263 = ORIENTED_EDGE ( 'NONE', *, *, #5155, .F. ) ;
#4264 = CARTESIAN_POINT ( 'NONE',  ( 2.765633920072239516, 21.30679549418631780, 12.59161484032919986 ) ) ;
#4265 = FACE_OUTER_BOUND ( 'NONE', #13894, .T. ) ;
#4266 = EDGE_CURVE ( 'NONE', #2063, #11374, #3105, .T. ) ;
#4267 = ORIENTED_EDGE ( 'NONE', *, *, #4323, .F. ) ;
#4268 = CARTESIAN_POINT ( 'NONE',  ( 2.789999999999999147, 0.2301004812057544924, 24.44424927289185590 ) ) ;
#4269 = EDGE_CURVE ( 'NONE', #9282, #497, #10165, .T. ) ;
#4270 = ORIENTED_EDGE ( 'NONE', *, *, #1734, .F. ) ;
#4271 = DIRECTION ( 'NONE',  ( -1.000000000000000000, -0.000000000000000000, -0.000000000000000000 ) ) ;
#4272 = CARTESIAN_POINT ( 'NONE',  ( 101.6227766016837819, -9.999999999999994671, 6.000000000000000000 ) ) ;
#4273 = ORIENTED_EDGE ( 'NONE', *, *, #1444, .F. ) ;
#4274 = CARTESIAN_POINT ( 'NONE',  ( 2.257825462012206685, 12.96514671151767395, 23.74442027961364943 ) ) ;
#4275 = LINE ( 'NONE', #14736, #10383 ) ;
#4276 = VERTEX_POINT ( 'NONE', #11317 ) ;
#4277 = ORIENTED_EDGE ( 'NONE', *, *, #11712, .F. ) ;
#4278 = CARTESIAN_POINT ( 'NONE',  ( 58.14665764790533586, -0.9105996816177498454, 4.000000000000000000 ) ) ;
#4279 = DIRECTION ( 'NONE',  ( 0.000000000000000000, 1.000000000000000000, -1.084202172485504187E-16 ) ) ;
#4280 = CARTESIAN_POINT ( 'NONE',  ( 2.789999999999999147, -20.70663861606260170, -15.04425356660783031 ) ) ;
#4281 = CARTESIAN_POINT ( 'NONE',  ( 2.764680872515353105, 13.68080036884348516, 5.229914364928400339 ) ) ;
#4282 = SHAPE_DEFINITION_REPRESENTATION ( #5673, #13067 ) ;
#4283 = CARTESIAN_POINT ( 'NONE',  ( 1.250000000000001110, 0.000000000000000000, 0.000000000000000000 ) ) ;
#4284 = CARTESIAN_POINT ( 'NONE',  ( 32.66827876307085887, -1.833751565556681173, -2.000000000000000888 ) ) ;
#4285 = DIRECTION ( 'NONE',  ( 1.000000000000000000, 0.000000000000000000, 0.000000000000000000 ) ) ;
#4286 = EDGE_LOOP ( 'NONE', ( #12799, #3243, #14483, #11996 ) ) ;
#4287 = DIRECTION ( 'NONE',  ( -1.000000000000000000, 0.000000000000000000, -0.000000000000000000 ) ) ;
#4288 = CYLINDRICAL_SURFACE ( 'NONE', #3985, 28.06981291497571362 ) ;
#4289 = VECTOR ( 'NONE', #6980, 1000.000000000000000 ) ;
#4290 = CARTESIAN_POINT ( 'NONE',  ( -1.150000000000000577, 7.225416114969384193E-16, 5.899999999999999467 ) ) ;
#4291 = ORIENTED_EDGE ( 'NONE', *, *, #1019, .T. ) ;
#4292 = CIRCLE ( 'NONE', #5036, 14.01039946648073986 ) ;
#4293 = EDGE_CURVE ( 'NONE', #14530, #10918, #9016, .T. ) ;
#4294 = CIRCLE ( 'NONE', #8210, 7.000000000000000000 ) ;
#4295 = DIRECTION ( 'NONE',  ( -1.000000000000000000, -0.000000000000000000, 0.000000000000000000 ) ) ;
#4296 = DIRECTION ( 'NONE',  ( 0.000000000000000000, 0.000000000000000000, 1.000000000000000000 ) ) ;
#4297 = ORIENTED_EDGE ( 'NONE', *, *, #4778, .T. ) ;
#4298 = ORIENTED_EDGE ( 'NONE', *, *, #1475, .T. ) ;
#4299 = DIRECTION ( 'NONE',  ( -1.000000000000000000, -0.000000000000000000, -0.000000000000000000 ) ) ;
#4300 = CYLINDRICAL_SURFACE ( 'NONE', #172, 4.000000000000000888 ) ;
#4301 = B_SPLINE_CURVE_WITH_KNOTS ( 'NONE', 3,
 ( #14464, #12053, #687, #4230 ),
 .UNSPECIFIED., .F., .F.,
 ( 4, 4 ),
 ( 0.005123695899043908056, 0.005814329666474863170 ),
 .UNSPECIFIED. ) ;
#4302 = CARTESIAN_POINT ( 'NONE',  ( -6.183853848222731672E-14, -14.05326139264729335, 2.096282088614720873 ) ) ;
#4303 = CARTESIAN_POINT ( 'NONE',  ( -4.872650870659752442, 0.4273491293402474911, -0.8000000000000000444 ) ) ;
#4304 = CARTESIAN_POINT ( 'NONE',  ( 0.006931054464086492187, 24.42321038836783131, 2.248820353273056405 ) ) ;
#4305 = CIRCLE ( 'NONE', #5779, 2.000000000000000000 ) ;
#4306 = EDGE_CURVE ( 'NONE', #6946, #7479, #7092, .T. ) ;
#4307 = EDGE_CURVE ( 'NONE', #3792, #11100, #7670, .T. ) ;
#4308 = CIRCLE ( 'NONE', #14117, 6.000000000000005329 ) ;
#4309 = DIRECTION ( 'NONE',  ( 0.000000000000000000, 0.000000000000000000, -1.000000000000000000 ) ) ;
#4310 = DIRECTION ( 'NONE',  ( -1.000000000000000000, 0.000000000000000000, -0.000000000000000000 ) ) ;
#4311 = VERTEX_POINT ( 'NONE', #2949 ) ;
#4312 = FACE_OUTER_BOUND ( 'NONE', #12524, .T. ) ;
#4313 = CARTESIAN_POINT ( 'NONE',  ( 2.764680872515352661, -2.311161484776655950, 14.46287784598616355 ) ) ;
#4314 = VERTEX_POINT ( 'NONE', #13778 ) ;
#4315 = CIRCLE ( 'NONE', #3808, 2.999999999999988898 ) ;
#4316 = FILL_AREA_STYLE ('',( #5630 ) ) ;
#4317 = AXIS2_PLACEMENT_3D ( 'NONE', #3770, #2404, #3862 ) ;
#4318 = ORIENTED_EDGE ( 'NONE', *, *, #5219, .F. ) ;
#4319 = ORIENTED_EDGE ( 'NONE', *, *, #9287, .T. ) ;
#4320 = EDGE_LOOP ( 'NONE', ( #2354, #7794, #7842, #9153 ) ) ;
#4321 = EDGE_CURVE ( 'NONE', #10385, #9762, #9622, .T. ) ;
#4322 = DIRECTION ( 'NONE',  ( 1.000000000000000000, 0.000000000000000000, 0.000000000000000000 ) ) ;
#4323 = EDGE_CURVE ( 'NONE', #6024, #1104, #15018, .T. ) ;
#4324 = CARTESIAN_POINT ( 'NONE',  ( 0.07186808533286581646, -23.19485392143207036, -10.24630254990540834 ) ) ;
#4325 = EDGE_CURVE ( 'NONE', #1482, #14436, #9385, .T. ) ;
#4326 = DIRECTION ( 'NONE',  ( -1.000000000000000000, 0.000000000000000000, 0.000000000000000000 ) ) ;
#4327 = VECTOR ( 'NONE', #6445, 1000.000000000000000 ) ;
#4328 = VERTEX_POINT ( 'NONE', #1018 ) ;
#4329 = CARTESIAN_POINT ( 'NONE',  ( 2.789999999999999147, 8.624777288397954322, -11.04103753892262496 ) ) ;
#4330 = CARTESIAN_POINT ( 'NONE',  ( 15.21482963846748504, 16.90833299098317610, -131.1575142076926852 ) ) ;
#4331 = ADVANCED_FACE ( 'NONE', ( #6866 ), #4243, .T. ) ;
#4332 = CARTESIAN_POINT ( 'NONE',  ( 0.8341317985991834050, 16.87476974924770801, 4.976599981640402071 ) ) ;
#4333 = CARTESIAN_POINT ( 'NONE',  ( 88.84370878116858705, 10.64188714589527507, 2.999999999999999112 ) ) ;
#4334 = AXIS2_PLACEMENT_3D ( 'NONE', #510, #6216, #282 ) ;
#4335 = ORIENTED_EDGE ( 'NONE', *, *, #12571, .F. ) ;
#4336 = CARTESIAN_POINT ( 'NONE',  ( -4.000000000000000000, 0.000000000000000000, 7.000000000000000000 ) ) ;
#4337 = CIRCLE ( 'NONE', #1633, 2.524999999999995914 ) ;
#4338 = CARTESIAN_POINT ( 'NONE',  ( -10.97587178374205941, -9.155129925568431304, -3.000000000000000444 ) ) ;
#4339 = ORIENTED_EDGE ( 'NONE', *, *, #11798, .F. ) ;
#4340 = ORIENTED_EDGE ( 'NONE', *, *, #8959, .T. ) ;
#4341 =( GEOMETRIC_REPRESENTATION_CONTEXT ( 3 ) GLOBAL_UNCERTAINTY_ASSIGNED_CONTEXT ( ( #11150 ) ) GLOBAL_UNIT_ASSIGNED_CONTEXT ( ( #15070, #12677, #6848 ) ) REPRESENTATION_CONTEXT ( 'NONE', 'WORKASPACE' ) );
#4342 = DIRECTION ( 'NONE',  ( -1.000000000000000000, -0.000000000000000000, -0.000000000000000000 ) ) ;
#4343 = VERTEX_POINT ( 'NONE', #1090 ) ;
#4344 = AXIS2_PLACEMENT_3D ( 'NONE', #12137, #5407, #8759 ) ;
#4345 = DIRECTION ( 'NONE',  ( -0.2314933715733012987, 0.9728364810787194505, 0.000000000000000000 ) ) ;
#4346 = EDGE_LOOP ( 'NONE', ( #10185, #5775, #13523, #5231 ) ) ;
#4347 = LINE ( 'NONE', #9034, #1858 ) ;
#4348 = CARTESIAN_POINT ( 'NONE',  ( 0.01818964989807676444, -13.58893811801117124, -5.219853812241048274 ) ) ;
#4349 = AXIS2_PLACEMENT_3D ( 'NONE', #12896, #11824, #289 ) ;
#4350 = ORIENTED_EDGE ( 'NONE', *, *, #3062, .F. ) ;
#4351 = CIRCLE ( 'NONE', #13671, 9.999999999999994671 ) ;
#4352 = DIRECTION ( 'NONE',  ( 0.000000000000000000, 0.3090169943749350723, 0.9510565162951576390 ) ) ;
#4353 = CARTESIAN_POINT ( 'NONE',  ( 0.7686372430964718561, 4.022333916463595394, 17.00993931356762801 ) ) ;
#4354 = VERTEX_POINT ( 'NONE', #12768 ) ;
#4355 = AXIS2_PLACEMENT_3D ( 'NONE', #12633, #14880, #12564 ) ;
#4356 = EDGE_LOOP ( 'NONE', ( #14181, #9341, #11503, #9338, #8459 ) ) ;
#4357 = B_SPLINE_CURVE_WITH_KNOTS ( 'NONE', 3,
 ( #8183, #11788, #2348, #3572, #2572, #11638, #14187, #14104 ),
 .UNSPECIFIED., .F., .F.,
 ( 4, 2, 2, 4 ),
 ( 4.663089341996299912E-07, 0.001898630032275737747, 0.002847711893946506829, 0.003796793755617275910 ),
 .UNSPECIFIED. ) ;
#4358 = DIRECTION ( 'NONE',  ( -1.000000000000000000, -0.000000000000000000, -0.000000000000000000 ) ) ;
#4359 = DIRECTION ( 'NONE',  ( -1.000000000000000000, 0.000000000000000000, 0.000000000000000000 ) ) ;
#4360 = AXIS2_PLACEMENT_3D ( 'NONE', #11510, #5686, #13751 ) ;
#4361 = CARTESIAN_POINT ( 'NONE',  ( 0.000000000000000000, 12.52067188844379864, -20.62201879784900882 ) ) ;
#4362 = CARTESIAN_POINT ( 'NONE',  ( 1.039999999999997149, -17.39253030560844948, 4.458161950358441317 ) ) ;
#4363 = CONTEXT_DEPENDENT_SHAPE_REPRESENTATION ( #14905, #2232 ) ;
#4364 = AXIS2_PLACEMENT_3D ( 'NONE', #10575, #7036, #11855 ) ;
#4365 = DIRECTION ( 'NONE',  ( 0.000000000000000000, 1.000000000000000000, 1.030528797609984825E-14 ) ) ;
#4366 = VECTOR ( 'NONE', #1357, 1000.000000000000000 ) ;
#4367 = VECTOR ( 'NONE', #5882, 1000.000000000000000 ) ;
#4368 = DIRECTION ( 'NONE',  ( -0.000000000000000000, -0.000000000000000000, 1.000000000000000000 ) ) ;
#4369 = ORIENTED_EDGE ( 'NONE', *, *, #10988, .F. ) ;
#4370 = LINE ( 'NONE', #673, #12233 ) ;
#4371 = CARTESIAN_POINT ( 'NONE',  ( 1.250000000000001110, 6.613092715395707467E-16, 5.400000000000000355 ) ) ;
#4372 = LINE ( 'NONE', #5678, #10484 ) ;
#4373 = ORIENTED_EDGE ( 'NONE', *, *, #1854, .F. ) ;
#4374 = AXIS2_PLACEMENT_3D ( 'NONE', #12982, #14145, #11902 ) ;
#4375 = LINE ( 'NONE', #7836, #14398 ) ;
#4377 = AXIS2_PLACEMENT_3D ( 'NONE', #7959, #8958, #2119 ) ;
#4376 = DIRECTION ( 'NONE',  ( -1.000000000000000000, -0.000000000000000000, -0.000000000000000000 ) ) ;
#4378 = EDGE_LOOP ( 'NONE', ( #4173, #2612, #4730, #11268 ) ) ;
#4379 = VECTOR ( 'NONE', #7935, 1000.000000000000000 ) ;
#4380 = ORIENTED_EDGE ( 'NONE', *, *, #6087, .T. ) ;
#4381 = DIRECTION ( 'NONE',  ( -5.339417856040273846E-17, -1.063174570779084847E-17, 1.000000000000000000 ) ) ;
#4382 = DIRECTION ( 'NONE',  ( 1.000000000000000000, 0.000000000000000000, 0.000000000000000000 ) ) ;
#4383 = EDGE_CURVE ( 'NONE', #13491, #8726, #3236, .T. ) ;
#4384 = VERTEX_POINT ( 'NONE', #13929 ) ;
#4385 = CARTESIAN_POINT ( 'NONE',  ( 83.50748565343083385, 13.38500995229612478, 4.000000000000000000 ) ) ;
#4386 = DIRECTION ( 'NONE',  ( -1.000000000000000000, 0.000000000000000000, -0.000000000000000000 ) ) ;
#4387 = CARTESIAN_POINT ( 'NONE',  ( -1.381028087215756681E-16, 24.22479935914660132, 2.133490293297101381 ) ) ;
#4388 = EDGE_CURVE ( 'NONE', #14287, #6222, #3008, .T. ) ;
#4389 = B_SPLINE_CURVE_WITH_KNOTS ( 'NONE', 3,
 ( #6173, #11920, #5033, #1410, #9555, #6100, #238, #5194 ),
 .UNSPECIFIED., .F., .F.,
 ( 4, 2, 2, 4 ),
 ( 4.663089412874008411E-07, 0.001898630173449118675, 0.002847712105703034072, 0.003796794037956949686 ),
 .UNSPECIFIED. ) ;
#4390 = AXIS2_PLACEMENT_3D ( 'NONE', #14534, #2994, #6530 ) ;
#4391 = CARTESIAN_POINT ( 'NONE',  ( 0.07186814640506919427, -12.74240566898967764, -21.92302674874977697 ) ) ;
#4392 = CARTESIAN_POINT ( 'NONE',  ( 0.000000000000000000, 15.74360496233383522, 18.28042085475283329 ) ) ;
#4393 = ORIENTED_EDGE ( 'NONE', *, *, #11078, .F. ) ;
#4394 = DIRECTION ( 'NONE',  ( 0.9021244663126474217, 0.4314758942051349910, -9.480662228539549174E-17 ) ) ;
#4395 = VECTOR ( 'NONE', #8941, 1000.000000000000000 ) ;
#4396 = AXIS2_PLACEMENT_3D ( 'NONE', #11420, #895, #4448 ) ;
#4397 = CARTESIAN_POINT ( 'NONE',  ( 65.21556745095632834, 33.50594455047664866, -2.000000000000000000 ) ) ;
#4398 = ORIENTED_EDGE ( 'NONE', *, *, #1732, .T. ) ;
#4399 = EDGE_CURVE ( 'NONE', #6867, #10187, #7639, .T. ) ;
#4400 = ADVANCED_FACE ( 'NONE', ( #10471 ), #12666, .T. ) ;
#4401 = VERTEX_POINT ( 'NONE', #11518 ) ;
#4402 = ORIENTED_EDGE ( 'NONE', *, *, #13612, .F. ) ;
#4403 = ORIENTED_EDGE ( 'NONE', *, *, #11078, .T. ) ;
#4404 = DIRECTION ( 'NONE',  ( 0.000000000000000000, 0.8090169943749400128, 0.5877852522924831291 ) ) ;
#4405 = FILL_AREA_STYLE_COLOUR ( '', #7798 ) ;
#4406 = DIRECTION ( 'NONE',  ( -1.000000000000000000, 0.000000000000000000, -0.000000000000000000 ) ) ;
#4407 =( REPRESENTATION_RELATIONSHIP ('NONE','NONE', #12685, #7891 ) REPRESENTATION_RELATIONSHIP_WITH_TRANSFORMATION ( #9276 )SHAPE_REPRESENTATION_RELATIONSHIP( ) );
#4408 = VECTOR ( 'NONE', #2809, 1000.000000000000000 ) ;
#4409 = VECTOR ( 'NONE', #11012, 1000.000000000000000 ) ;
#4410 = TOROIDAL_SURFACE ( 'NONE', #4163, 24.12539914357697768, 8.000000000000000000 ) ;
#4411 = LINE ( 'NONE', #10240, #1966 ) ;
#4412 = VERTEX_POINT ( 'NONE', #11369 ) ;
#4413 = CARTESIAN_POINT ( 'NONE',  ( 2.789999999999999147, 5.249430348645756084, 12.98979500319695823 ) ) ;
#4414 = CARTESIAN_POINT ( 'NONE',  ( 2.789999999999999147, 20.62201879784931435, -12.52067188844328882 ) ) ;
#4415 = ADVANCED_FACE ( 'NONE', ( #6689 ), #6841, .F. ) ;
#4416 = B_SPLINE_CURVE_WITH_KNOTS ( 'NONE', 3,
 ( #3819, #9430, #11878, #9362 ),
 .UNSPECIFIED., .F., .F.,
 ( 4, 4 ),
 ( 2.451234579310872104E-07, 0.0006917187676826484820 ),
 .UNSPECIFIED. ) ;
#4417 = AXIS2_PLACEMENT_3D ( 'NONE', #15063, #4309, #1929 ) ;
#4418 = CARTESIAN_POINT ( 'NONE',  ( 75.68384697807671557, 11.35494834827056110, -2.000000000000000888 ) ) ;
#4419 = EDGE_CURVE ( 'NONE', #8921, #4328, #14615, .T. ) ;
#4420 = VERTEX_POINT ( 'NONE', #839 ) ;
#4421 = CARTESIAN_POINT ( 'NONE',  ( 1.394999999999998685, -27.68468304288255410, -4.633866840649221608 ) ) ;
#4422 = DIRECTION ( 'NONE',  ( -1.000000000000000000, 0.000000000000000000, 0.000000000000000000 ) ) ;
#4423 = ORIENTED_EDGE ( 'NONE', *, *, #1489, .F. ) ;
#4424 = ORIENTED_EDGE ( 'NONE', *, *, #5646, .T. ) ;
#4425 = EDGE_CURVE ( 'NONE', #10003, #6544, #1593, .T. ) ;
#4426 = SURFACE_SIDE_STYLE ('',( #2029 ) ) ;
#4427 = CARTESIAN_POINT ( 'NONE',  ( 80.00000000000000000, 0.000000000000000000, 6.000000000000000000 ) ) ;
#4428 = VECTOR ( 'NONE', #4368, 1000.000000000000000 ) ;
#4429 = VERTEX_POINT ( 'NONE', #4392 ) ;
#4430 = CARTESIAN_POINT ( 'NONE',  ( 19.25177984293775069, 7.759396820770414926, 6.000000000000000000 ) ) ;
#4431 = CARTESIAN_POINT ( 'NONE',  ( 2.764680872515353105, 13.68080036884348516, 5.229914364928400339 ) ) ;
#4432 = CARTESIAN_POINT ( 'NONE',  ( 2.765633920072238183, 2.336989772644269436, 24.63872515616083447 ) ) ;
#4433 = VERTEX_POINT ( 'NONE', #15064 ) ;
#4434 = PRESENTATION_STYLE_ASSIGNMENT (( #9039 ) ) ;
#4435 = CARTESIAN_POINT ( 'NONE',  ( -1.150000000000001688, 0.000000000000000000, 0.000000000000000000 ) ) ;
#4436 = ORIENTED_EDGE ( 'NONE', *, *, #8997, .F. ) ;
#4437 = ORIENTED_EDGE ( 'NONE', *, *, #14756, .F. ) ;
#4438 = PLANE ( 'NONE',  #4862 ) ;
#4439 = PLANE ( 'NONE',  #14685 ) ;
#4440 = EDGE_CURVE ( 'NONE', #2255, #14957, #693, .T. ) ;
#4441 = CYLINDRICAL_SURFACE ( 'NONE', #9972, 4.999999999999997335 ) ;
#4442 = CARTESIAN_POINT ( 'NONE',  ( 1.039999999999996927, -4.633866840649124796, 27.68468304288256832 ) ) ;
#4443 = ITEM_DEFINED_TRANSFORMATION ( 'NONE', 'NONE', #7943,  #1376 ) ;
#4444 = CARTESIAN_POINT ( 'NONE',  ( 2.783068945535915883, -2.248820353272798389, -24.42321038836784908 ) ) ;
#4445 = PRODUCT_DEFINITION_SHAPE ( 'NONE', 'NONE',  #15241 ) ;
#4446 = CARTESIAN_POINT ( 'NONE',  ( 1.039999999999996261, 24.89775460606850999, -12.96210679857759018 ) ) ;
#4447 = ORIENTED_EDGE ( 'NONE', *, *, #12943, .F. ) ;
#4448 = DIRECTION ( 'NONE',  ( 0.000000000000000000, 0.000000000000000000, 1.000000000000000000 ) ) ;
#4449 = CARTESIAN_POINT ( 'NONE',  ( -10.00000000000000000, 0.000000000000000000, 0.000000000000000000 ) ) ;
#4450 = DIRECTION ( 'NONE',  ( 1.000000000000000000, 0.000000000000000000, 0.000000000000000000 ) ) ;
#4451 = ADVANCED_FACE ( 'NONE', ( #10300 ), #13827, .F. ) ;
#4452 = ORIENTED_EDGE ( 'NONE', *, *, #7849, .T. ) ;
#4453 = EDGE_CURVE ( 'NONE', #12548, #316, #2869, .T. ) ;
#4454 = DIRECTION ( 'NONE',  ( -1.000000000000000000, -0.000000000000000000, -0.000000000000000000 ) ) ;
#4455 = CARTESIAN_POINT ( 'NONE',  ( -7.841635642041319107E-14, -15.96555658743749717, -18.34439787333524663 ) ) ;
#4456 = ORIENTED_EDGE ( 'NONE', *, *, #12002, .T. ) ;
#4457 = ORIENTED_EDGE ( 'NONE', *, *, #3095, .F. ) ;
#4458 = DIRECTION ( 'NONE',  ( -1.000000000000000000, -0.000000000000000000, -0.000000000000000000 ) ) ;
#4459 = DIRECTION ( 'NONE',  ( 1.000000000000000000, 0.000000000000000000, 0.000000000000000000 ) ) ;
#4460 = ORIENTED_EDGE ( 'NONE', *, *, #7701, .F. ) ;
#4461 = CARTESIAN_POINT ( 'NONE',  ( 2.783025306068356297, 16.17543236988015209, -18.43727551351014071 ) ) ;
#4462 = LINE ( 'NONE', #5761, #5528 ) ;
#4463 = CARTESIAN_POINT ( 'NONE',  ( 60.61028236725008611, -31.15713940066885712, 6.000000000000000000 ) ) ;
#4464 = CARTESIAN_POINT ( 'NONE',  ( 1.039999999999995373, -12.96210679857767900, -24.89775460606846380 ) ) ;
#4465 = DIRECTION ( 'NONE',  ( 0.000000000000000000, 0.000000000000000000, 1.000000000000000000 ) ) ;
#4466 = EDGE_CURVE ( 'NONE', #10187, #12893, #12396, .T. ) ;
#4467 = ORIENTED_EDGE ( 'NONE', *, *, #4195, .F. ) ;
#4468 = CARTESIAN_POINT ( 'NONE',  ( 2.246812880117043498, 16.57708379306443902, 3.619024283482126680 ) ) ;
#4469 = DIRECTION ( 'NONE',  ( 0.000000000000000000, 0.000000000000000000, -1.000000000000000000 ) ) ;
#4470 = EDGE_CURVE ( 'NONE', #10878, #134, #995, .T. ) ;
#4471 = ORIENTED_EDGE ( 'NONE', *, *, #10432, .F. ) ;
#4472 = VERTEX_POINT ( 'NONE', #13681 ) ;
#4473 = EDGE_LOOP ( 'NONE', ( #9850, #4491, #14840, #13950, #2304, #14737 ) ) ;
#4474 = VERTEX_POINT ( 'NONE', #6534 ) ;
#4475 = DIRECTION ( 'NONE',  ( 0.000000000000000000, 0.000000000000000000, 1.000000000000000000 ) ) ;
#4476 = AXIS2_PLACEMENT_3D ( 'NONE', #9130, #13812, #1990 ) ;
#4477 = FACE_OUTER_BOUND ( 'NONE', #6462, .T. ) ;
#4478 = UNCERTAINTY_MEASURE_WITH_UNIT (LENGTH_MEASURE( 1.000000000000000082E-05 ), #4767, 'distance_accuracy_value', 'NONE');
#4479 = LINE ( 'NONE', #9160, #6865 ) ;
#4480 = EDGE_CURVE ( 'NONE', #2078, #3198, #7919, .T. ) ;
#4481 = ORIENTED_EDGE ( 'NONE', *, *, #12890, .F. ) ;
#4482 = DIRECTION ( 'NONE',  ( 1.000000000000000000, 0.000000000000000000, 0.000000000000000000 ) ) ;
#4483 = CARTESIAN_POINT ( 'NONE',  ( 0.7592463896980138349, 19.86438386685688684, -19.12676442129323107 ) ) ;
#4484 = CIRCLE ( 'NONE', #6438, 3.000000000000002665 ) ;
#4485 = CARTESIAN_POINT ( 'NONE',  ( 2.783068961317272549, 21.08061549536614976, 12.53626894672835945 ) ) ;
#4486 = EDGE_CURVE ( 'NONE', #13724, #14414, #12366, .T. ) ;
#4487 = ORIENTED_EDGE ( 'NONE', *, *, #14935, .T. ) ;
#4488 = B_SPLINE_CURVE_WITH_KNOTS ( 'NONE', 3,
 ( #5934, #7231, #14148, #12985, #9535, #2473, #3690, #11906 ),
 .UNSPECIFIED., .F., .F.,
 ( 4, 2, 2, 4 ),
 ( 2.154797737779095183E-07, 0.001895231411415135075, 0.002842739377235819782, 0.003790247343056505139 ),
 .UNSPECIFIED. ) ;
#4489 = CARTESIAN_POINT ( 'NONE',  ( 80.82762530298222714, -19.99999999999999645, -130.1575142076926852 ) ) ;
#4490 = DIRECTION ( 'NONE',  ( 0.000000000000000000, 0.000000000000000000, 1.000000000000000000 ) ) ;
#4491 = ORIENTED_EDGE ( 'NONE', *, *, #10695, .F. ) ;
#4492 = VERTEX_POINT ( 'NONE', #10073 ) ;
#4493 = AXIS2_PLACEMENT_3D ( 'NONE', #14769, #7991, #4465 ) ;
#4494 = DIRECTION ( 'NONE',  ( -1.000000000000000000, -0.000000000000000000, -0.000000000000000000 ) ) ;
#4495 = EDGE_CURVE ( 'NONE', #11120, #6334, #8910, .T. ) ;
#4496 = ADVANCED_FACE ( 'NONE', ( #2153 ), #14999, .F. ) ;
#4497 = ORIENTED_EDGE ( 'NONE', *, *, #12434, .F. ) ;
#4498 = CYLINDRICAL_SURFACE ( 'NONE', #9794, 3.799999999999999378 ) ;
#4499 = DIRECTION ( 'NONE',  ( -0.9873505073845697533, 0.1585527532634883052, 0.000000000000000000 ) ) ;
#4500 = CYLINDRICAL_SURFACE ( 'NONE', #3536, 20.00000000000000000 ) ;
#4501 = ORIENTED_EDGE ( 'NONE', *, *, #13692, .F. ) ;
#4502 = FACE_OUTER_BOUND ( 'NONE', #7611, .T. ) ;
#4503 = CARTESIAN_POINT ( 'NONE',  ( 0.2076373213219092628, 2.899259574942746998, 15.57879356040263907 ) ) ;
#4504 = ORIENTED_EDGE ( 'NONE', *, *, #1093, .T. ) ;
#4505 = VERTEX_POINT ( 'NONE', #12742 ) ;
#4506 = ADVANCED_FACE ( 'NONE', ( #3449 ), #11588, .F. ) ;
#4507 = LINE ( 'NONE', #12569, #4120 ) ;
#4508 = DIRECTION ( 'NONE',  ( -1.000000000000000000, -0.000000000000000000, -0.000000000000000000 ) ) ;
#4509 = EDGE_CURVE ( 'NONE', #11060, #5604, #13034, .T. ) ;
#4510 = CARTESIAN_POINT ( 'NONE',  ( 1.000000000000000000, -5.408326913195983465, -0.8000000000000000444 ) ) ;
#4511 = DIRECTION ( 'NONE',  ( -1.000000000000000000, 0.000000000000000000, 0.000000000000000000 ) ) ;
#4512 = CARTESIAN_POINT ( 'NONE',  ( 2.765633920072235519, -18.55949924794880346, -16.37294372382878649 ) ) ;
#4513 = EDGE_CURVE ( 'NONE', #6024, #7008, #4165, .T. ) ;
#4514 = CARTESIAN_POINT ( 'NONE',  ( -19.40394475573011590, -4.794738323547945491, 16.99999999999999645 ) ) ;
#4515 = ORIENTED_EDGE ( 'NONE', *, *, #5177, .F. ) ;
#4516 = DIRECTION ( 'NONE',  ( -1.000000000000000000, 0.000000000000000000, -0.000000000000000000 ) ) ;
#4517 = DIRECTION ( 'NONE',  ( 0.000000000000000000, 0.000000000000000000, 1.000000000000000000 ) ) ;
#4518 = B_SPLINE_CURVE_WITH_KNOTS ( 'NONE', 3,
 ( #9492, #9345, #6034, #7187 ),
 .UNSPECIFIED., .F., .F.,
 ( 4, 4 ),
 ( 3.059063720760159520E-07, 0.0006888942284914070097 ),
 .UNSPECIFIED. ) ;
#4519 = CYLINDRICAL_SURFACE ( 'NONE', #12450, 2.524999999999995914 ) ;
#4520 = ADVANCED_FACE ( 'NONE', ( #15144 ), #6199, .T. ) ;
#4521 = AXIS2_PLACEMENT_3D ( 'NONE', #7136, #13270, #14207 ) ;
#4522 = VERTEX_POINT ( 'NONE', #5762 ) ;
#4523 = CARTESIAN_POINT ( 'NONE',  ( -12.16787677823033142, -13.79473832354794993, 14.99999999999999822 ) ) ;
#4524 = CARTESIAN_POINT ( 'NONE',  ( -16.92833982302709828, -13.89754826684236200, 0.7999999999999960476 ) ) ;
#4525 = VECTOR ( 'NONE', #5265, 1000.000000000000000 ) ;
#4526 = VERTEX_POINT ( 'NONE', #9516 ) ;
#4527 = VECTOR ( 'NONE', #11071, 1000.000000000000000 ) ;
#4528 = ORIENTED_EDGE ( 'NONE', *, *, #12744, .T. ) ;
#4529 = DIRECTION ( 'NONE',  ( -1.000000000000000000, 0.000000000000000000, 0.000000000000000000 ) ) ;
#4530 = DIRECTION ( 'NONE',  ( 0.000000000000000000, 0.000000000000000000, 1.000000000000000000 ) ) ;
#4531 = ORIENTED_EDGE ( 'NONE', *, *, #10879, .F. ) ;
#4532 = AXIS2_PLACEMENT_3D ( 'NONE', #14674, #8966, #9974 ) ;
#4533 = CARTESIAN_POINT ( 'NONE',  ( 1.885839517048287561, -17.20101185194003790, 4.239993951493146618 ) ) ;
#4534 = DIRECTION ( 'NONE',  ( -0.000000000000000000, -0.000000000000000000, 1.000000000000000000 ) ) ;
#4535 = CARTESIAN_POINT ( 'NONE',  ( 1.749999999999998002, 4.633866840648922292, 27.68468304288260384 ) ) ;
#4536 = CARTESIAN_POINT ( 'NONE',  ( 2.789999999999999147, -1.991882183130126549, -24.04302995059967429 ) ) ;
#4537 = DIRECTION ( 'NONE',  ( -0.000000000000000000, -0.000000000000000000, 1.000000000000000000 ) ) ;
#4538 = CIRCLE ( 'NONE', #13098, 28.06981291497571362 ) ;
#4539 = ORIENTED_EDGE ( 'NONE', *, *, #7931, .F. ) ;
#4540 = FACE_OUTER_BOUND ( 'NONE', #5889, .T. ) ;
#4541 = VECTOR ( 'NONE', #1564, 1000.000000000000000 ) ;
#4542 = TOROIDAL_SURFACE ( 'NONE', #8451, 24.12539914357697413, 8.000000000000000000 ) ;
#4543 = LINE ( 'NONE', #5771, #5269 ) ;
#4544 = ORIENTED_EDGE ( 'NONE', *, *, #817, .F. ) ;
#4545 = ADVANCED_FACE ( 'NONE', ( #45, #8357 ), #8067, .T. ) ;
#4546 =( NAMED_UNIT ( * ) PLANE_ANGLE_UNIT ( ) SI_UNIT ( $, .RADIAN. ) );
#4547 = VERTEX_POINT ( 'NONE', #1222 ) ;
#4548 = VERTEX_POINT ( 'NONE', #11808 ) ;
#4549 = VERTEX_POINT ( 'NONE', #7137 ) ;
#4550 = CARTESIAN_POINT ( 'NONE',  ( -14.40394475573011945, -10.79473832354794460, -5.000000000000000000 ) ) ;
#4551 = CIRCLE ( 'NONE', #2084, 3.799999999999998934 ) ;
#4552 = AXIS2_PLACEMENT_3D ( 'NONE', #12611, #3250, #9011 ) ;
#4553 = CARTESIAN_POINT ( 'NONE',  ( 0.1855654851361725199, -23.63475234378974577, -10.67816411292190004 ) ) ;
#4554 = CARTESIAN_POINT ( 'NONE',  ( 2.764680872515353993, -5.229914364928256454, -13.68080036884353845 ) ) ;
#4555 = CARTESIAN_POINT ( 'NONE',  ( 13.28797974610714761, -21.11867004231547540, -131.1575142076926852 ) ) ;
#4556 = EDGE_CURVE ( 'NONE', #7436, #2289, #13556, .T. ) ;
#4557 = DIRECTION ( 'NONE',  ( -5.480158469902919838E-17, -1.051478716308701618E-16, -1.000000000000000000 ) ) ;
#4558 = ORIENTED_EDGE ( 'NONE', *, *, #11818, .F. ) ;
#4559 = CARTESIAN_POINT ( 'NONE',  ( 1.039999999999997371, 25.12109765559653596, 12.52377138324232675 ) ) ;
#4560 = CIRCLE ( 'NONE', #8707, 14.01039946648074341 ) ;
#4561 = VECTOR ( 'NONE', #705, 1000.000000000000000 ) ;
#4562 = VECTOR ( 'NONE', #2712, 1000.000000000000000 ) ;
#4563 = CARTESIAN_POINT ( 'NONE',  ( 0.04999671152044155020, 14.75565684666100275, -2.439987328296890468 ) ) ;
#4564 = ORIENTED_EDGE ( 'NONE', *, *, #1070, .F. ) ;
#4565 = CARTESIAN_POINT ( 'NONE',  ( 60.64109936584995353, 31.48746944824151583, 2.000000000000000000 ) ) ;
#4566 = PRODUCT_DEFINITION_SHAPE ( 'NONE', 'NONE',  #15230 ) ;
#4567 = DIRECTION ( 'NONE',  ( -0.4036950204470272086, 0.9148936170212765839, 0.000000000000000000 ) ) ;
#4568 = ORIENTED_EDGE ( 'NONE', *, *, #6748, .T. ) ;
#4569 = ORIENTED_EDGE ( 'NONE', *, *, #1156, .T. ) ;
#4570 = EDGE_CURVE ( 'NONE', #14075, #12114, #8891, .T. ) ;
#4571 = DIRECTION ( 'NONE',  ( 1.576560579138138762E-17, -1.359337748750801762E-17, 1.000000000000000000 ) ) ;
#4572 = ORIENTED_EDGE ( 'NONE', *, *, #4307, .T. ) ;
#4573 = CARTESIAN_POINT ( 'NONE',  ( 8.000000000000000000, 0.000000000000000000, 0.000000000000000000 ) ) ;
#4574 = EDGE_CURVE ( 'NONE', #6094, #5377, #2269, .T. ) ;
#4575 = CARTESIAN_POINT ( 'NONE',  ( 1.749999999999999778, 0.000000000000000000, 0.000000000000000000 ) ) ;
#4576 = CARTESIAN_POINT ( 'NONE',  ( 2.765633920072235519, 24.15498966839970052, -5.391175441198366336 ) ) ;
#4577 = TOROIDAL_SURFACE ( 'NONE', #13148, 14.01039946648073986, 8.000000000000000000 ) ;
#4578 = DIRECTION ( 'NONE',  ( 0.000000000000000000, 0.000000000000000000, 1.000000000000000000 ) ) ;
#4579 = ORIENTED_EDGE ( 'NONE', *, *, #8638, .T. ) ;
#4580 = VECTOR ( 'NONE', #1611, 1000.000000000000000 ) ;
#4581 = DIRECTION ( 'NONE',  ( 0.6743761619433820131, 0.7383879686198261405, -5.947623346206184252E-19 ) ) ;
#4582 = CARTESIAN_POINT ( 'NONE',  ( 2.782672486186223981, -13.44898112152242220, 5.204526028255641812 ) ) ;
#4583 =( GEOMETRIC_REPRESENTATION_CONTEXT ( 3 ) GLOBAL_UNCERTAINTY_ASSIGNED_CONTEXT ( ( #3946 ) ) GLOBAL_UNIT_ASSIGNED_CONTEXT ( ( #1883, #12487, #10101 ) ) REPRESENTATION_CONTEXT ( 'NONE', 'WORKASPACE' ) );
#4584 = EDGE_LOOP ( 'NONE', ( #9033, #11682, #11208, #14116, #11428, #13711, #10453, #2167 ) ) ;
#4585 = PRODUCT_RELATED_PRODUCT_CATEGORY ( 'part', '', ( #14008 ) ) ;
#4586 = EDGE_CURVE ( 'NONE', #5643, #5736, #8157, .T. ) ;
#4587 = EDGE_CURVE ( 'NONE', #4311, #5498, #11619, .T. ) ;
#4588 = VERTEX_POINT ( 'NONE', #8203 ) ;
#4589 = CARTESIAN_POINT ( 'NONE',  ( 2.789999999999999147, 14.46287784598617243, 2.311161484776605324 ) ) ;
#4590 = DIRECTION ( 'NONE',  ( 0.000000000000000000, 6.870191984066565499E-15, -1.000000000000000000 ) ) ;
#4591 = VECTOR ( 'NONE', #4787, 1000.000000000000000 ) ;
#4592 = CARTESIAN_POINT ( 'NONE',  ( 2.789999999999999147, 16.37294372382885044, -18.55949924794875017 ) ) ;
#4593 = CARTESIAN_POINT ( 'NONE',  ( -14.40394475573011945, -10.79473832354794460, 0.7999999999999960476 ) ) ;
#4594 = CARTESIAN_POINT ( 'NONE',  ( -1.150000000000001688, 0.000000000000000000, 0.000000000000000000 ) ) ;
#4595 = CIRCLE ( 'NONE', #4093, 11.66666666666667318 ) ;
#4596 = AXIS2_PLACEMENT_3D ( 'NONE', #13128, #57, #2469 ) ;
#4597 = CARTESIAN_POINT ( 'NONE',  ( -7.940452095251188120E-14, -18.34439787333518268, 15.96555658743757000 ) ) ;
#4598 = AXIS2_PLACEMENT_3D ( 'NONE', #8034, #15196, #9340 ) ;
#4599 = ORIENTED_EDGE ( 'NONE', *, *, #9349, .T. ) ;
#4600 = CARTESIAN_POINT ( 'NONE',  ( 2.790000000000000036, 22.37986894186685660, -9.514945144208509120 ) ) ;
#4601 = DIRECTION ( 'NONE',  ( 0.000000000000000000, 0.000000000000000000, 1.000000000000000000 ) ) ;
#4602 = DIRECTION ( 'NONE',  ( 0.000000000000000000, 0.000000000000000000, 1.000000000000000000 ) ) ;
#4603 = CARTESIAN_POINT ( 'NONE',  ( 2.764680872515352661, 5.229914364928351489, 13.68080036884350292 ) ) ;
#4604 = EDGE_CURVE ( 'NONE', #11133, #13658, #13056, .T. ) ;
#4605 = CIRCLE ( 'NONE', #14902, 4.599999999999999645 ) ;
#4606 = EDGE_LOOP ( 'NONE', ( #4218, #8293, #2379, #5675 ) ) ;
#4607 = EDGE_CURVE ( 'NONE', #9067, #4798, #10194, .T. ) ;
#4608 = CARTESIAN_POINT ( 'NONE',  ( 2.789999999999999147, -20.70663861606282197, 15.04425356660753188 ) ) ;
#4609 = CARTESIAN_POINT ( 'NONE',  ( 2.765633920072242180, 22.71065055754465689, -9.836394144775473691 ) ) ;
#4610 = ORIENTED_EDGE ( 'NONE', *, *, #1916, .T. ) ;
#4611 = B_SPLINE_CURVE_WITH_KNOTS ( 'NONE', 3,
 ( #14193, #3579, #8266, #9578, #11863, #10647 ),
 .UNSPECIFIED., .F., .F.,
 ( 4, 2, 4 ),
 ( 4.462636793144857890E-07, 0.001879885123570645663, 0.003759323983461976531 ),
 .UNSPECIFIED. ) ;
#4612 = VECTOR ( 'NONE', #13648, 1000.000000000000000 ) ;
#4613 = VERTEX_POINT ( 'NONE', #117 ) ;
#4614 = AXIS2_PLACEMENT_3D ( 'NONE', #11514, #2224, #8984 ) ;
#4615 = CARTESIAN_POINT ( 'NONE',  ( 0.002676282549904213624, -13.26666194250858233, -5.214906618938926819 ) ) ;
#4616 = CYLINDRICAL_SURFACE ( 'NONE', #8537, 17.95481323787947403 ) ;
#4617 = VERTEX_POINT ( 'NONE', #9363 ) ;
#4618 = TOROIDAL_SURFACE ( 'NONE', #10732, 24.12539914357697768, 8.000000000000000000 ) ;
#4619 = CARTESIAN_POINT ( 'NONE',  ( 0.02531912748464718033, -14.46287784598619020, 2.311161484776505404 ) ) ;
#4620 = DIRECTION ( 'NONE',  ( 2.081668171172168513E-16, -1.000000000000000000, 0.000000000000000000 ) ) ;
#4621 = CARTESIAN_POINT ( 'NONE',  ( 84.00000000000000000, 0.000000000000000000, -130.1575142076926852 ) ) ;
#4622 = EDGE_CURVE ( 'NONE', #11374, #12104, #469, .T. ) ;
#4623 = FACE_OUTER_BOUND ( 'NONE', #11601, .T. ) ;
#4624 = FACE_OUTER_BOUND ( 'NONE', #10284, .T. ) ;
#4625 = ORIENTED_EDGE ( 'NONE', *, *, #6578, .T. ) ;
#4626 = DIRECTION ( 'NONE',  ( -0.000000000000000000, -0.000000000000000000, 1.000000000000000000 ) ) ;
#4627 = CIRCLE ( 'NONE', #4135, 4.100000000000000533 ) ;
#4628 = DIRECTION ( 'NONE',  ( -1.000000000000000000, -0.000000000000000000, -0.000000000000000000 ) ) ;
#4629 = TOROIDAL_SURFACE ( 'NONE', #8046, 24.12539914357697768, 8.000000000000000000 ) ;
#4630 = ORIENTED_EDGE ( 'NONE', *, *, #13966, .T. ) ;
#4631 = AXIS2_PLACEMENT_3D ( 'NONE', #2461, #3679, #5712 ) ;
#4632 = DIRECTION ( 'NONE',  ( 1.000000000000000000, 0.000000000000000000, 0.000000000000000000 ) ) ;
#4633 = ORIENTED_EDGE ( 'NONE', *, *, #14894, .T. ) ;
#4634 = ORIENTED_EDGE ( 'NONE', *, *, #12683, .F. ) ;
#4635 = ORIENTED_EDGE ( 'NONE', *, *, #4019, .T. ) ;
#4636 = DIRECTION ( 'NONE',  ( -1.000000000000000000, 0.000000000000000000, -0.000000000000000000 ) ) ;
#4637 = CARTESIAN_POINT ( 'NONE',  ( 2.765633920072242624, 9.836394144775706394, 22.71065055754456097 ) ) ;
#4638 = AXIS2_PLACEMENT_3D ( 'NONE', #8793, #3315, #642 ) ;
#4639 = CARTESIAN_POINT ( 'NONE',  ( 0.02531912748464718033, -9.232963481057685939, -11.36963888406697087 ) ) ;
#4640 = DIRECTION ( 'NONE',  ( 0.000000000000000000, 0.000000000000000000, 1.000000000000000000 ) ) ;
#4641 = CARTESIAN_POINT ( 'NONE',  ( 0.2818303507154722998, -3.072260951847419097, -15.84037596932111036 ) ) ;
#4642 = TOROIDAL_SURFACE ( 'NONE', #6343, 24.12539914357697768, 8.000000000000000000 ) ;
#4643 = VECTOR ( 'NONE', #14575, 1000.000000000000114 ) ;
#4644 = ORIENTED_EDGE ( 'NONE', *, *, #1583, .T. ) ;
#4645 = DIRECTION ( 'NONE',  ( 1.000000000000000000, -0.000000000000000000, 0.000000000000000000 ) ) ;
#4646 = CARTESIAN_POINT ( 'NONE',  ( 2.790000000000000036, 20.85230829256853013, 12.51294990530023732 ) ) ;
#4647 = AXIS2_PLACEMENT_3D ( 'NONE', #14344, #3807, #14508 ) ;
#4648 = AXIS2_PLACEMENT_3D ( 'NONE', #4268, #10260, #14961 ) ;
#4649 = ORIENTED_EDGE ( 'NONE', *, *, #1583, .F. ) ;
#4650 = CARTESIAN_POINT ( 'NONE',  ( -10.40394475573011945, -10.79473832354794460, 0.7999999999999959366 ) ) ;
#4651 = CARTESIAN_POINT ( 'NONE',  ( 2.782650442329440477, 11.23191127083875962, -9.045126717605661781 ) ) ;
#4652 = EDGE_CURVE ( 'NONE', #6129, #15110, #3593, .T. ) ;
#4653 = ORIENTED_EDGE ( 'NONE', *, *, #14230, .T. ) ;
#4654 = VERTEX_POINT ( 'NONE', #10663 ) ;
#4655 = PLANE ( 'NONE',  #2092 ) ;
#4656 = ORIENTED_EDGE ( 'NONE', *, *, #4177, .T. ) ;
#4657 = CARTESIAN_POINT ( 'NONE',  ( 0.02436607992776151574, 24.15498966839970052, -5.391175441198366336 ) ) ;
#4658 = CARTESIAN_POINT ( 'NONE',  ( 0.006974674093432157128, -2.249040938978327908, -24.42374957165208116 ) ) ;
#4659 = TOROIDAL_SURFACE ( 'NONE', #14964, 14.01039946648073986, 8.000000000000000000 ) ;
#4660 = ADVANCED_FACE ( 'NONE', ( #3821 ), #10747, .T. ) ;
#4661 = CARTESIAN_POINT ( 'NONE',  ( 0.04387302227425587953, -0.8988970056815600573, 6.000000000000000000 ) ) ;
#4662 = CARTESIAN_POINT ( 'NONE',  ( 72.68384697807672978, 11.35494834827056110, 4.000000000000000000 ) ) ;
#4663 = VERTEX_POINT ( 'NONE', #10889 ) ;
#4664 = DIRECTION ( 'NONE',  ( 0.000000000000000000, 6.870191984066573782E-16, -1.000000000000000000 ) ) ;
#4665 = EDGE_CURVE ( 'NONE', #8012, #9282, #14444, .T. ) ;
#4666 = CARTESIAN_POINT ( 'NONE',  ( 0.9041604829517113640, 4.239993951493447710, -17.20101185193995974 ) ) ;
#4667 = VERTEX_POINT ( 'NONE', #7288 ) ;
#4668 = EDGE_CURVE ( 'NONE', #8109, #10680, #9823, .T. ) ;
#4669 = EDGE_LOOP ( 'NONE', ( #13024, #1176, #12087, #4934 ) ) ;
#4670 = DIRECTION ( 'NONE',  ( -0.4036950204470279302, 0.9148936170212763619, 0.000000000000000000 ) ) ;
#4671 = VECTOR ( 'NONE', #6930, 1000.000000000000114 ) ;
#4672 = CARTESIAN_POINT ( 'NONE',  ( -1.398397006336996817, -6.091550361990593743, 0.000000000000000000 ) ) ;
#4673 = DIRECTION ( 'NONE',  ( -0.9237280213470681067, -0.3830490080632377725, 0.000000000000000000 ) ) ;
#4674 = CARTESIAN_POINT ( 'NONE',  ( -7.372183127218402931E-16, -20.85230829256862961, 12.51294990530008988 ) ) ;
#4675 = FACE_OUTER_BOUND ( 'NONE', #13775, .T. ) ;
#4676 = CARTESIAN_POINT ( 'NONE',  ( 1.394999999999999574, -12.52377138324206740, -25.12109765559666741 ) ) ;
#4677 = EDGE_CURVE ( 'NONE', #2043, #12774, #12749, .T. ) ;
#4678 = VERTEX_POINT ( 'NONE', #4994 ) ;
#4679 = DIRECTION ( 'NONE',  ( 1.000000000000000000, 0.000000000000000000, 0.000000000000000000 ) ) ;
#4680 = DIRECTION ( 'NONE',  ( 0.000000000000000000, 0.000000000000000000, 1.000000000000000000 ) ) ;
#4681 = CARTESIAN_POINT ( 'NONE',  ( -5.209999999999999964, 0.000000000000000000, 0.000000000000000000 ) ) ;
#4682 = AXIS2_PLACEMENT_3D ( 'NONE', #1365, #11591, #5764 ) ;
#4683 = CARTESIAN_POINT ( 'NONE',  ( 1.749999999999998002, -4.147968289691484678, 27.76164181293050603 ) ) ;
#4684 = ORIENTED_EDGE ( 'NONE', *, *, #5091, .T. ) ;
#4685 = B_SPLINE_CURVE_WITH_KNOTS ( 'NONE', 3,
 ( #11700, #1034, #7104, #10402, #1187, #3338, #13864, #8326 ),
 .UNSPECIFIED., .F., .F.,
 ( 4, 2, 2, 4 ),
 ( 4.663089341997027831E-07, 0.001440500229357419932, 0.002160517189569030432, 0.002880534149780641148 ),
 .UNSPECIFIED. ) ;
#4686 = ORIENTED_EDGE ( 'NONE', *, *, #13956, .F. ) ;
#4687 = EDGE_CURVE ( 'NONE', #9975, #4667, #2028, .T. ) ;
#4688 = ORIENTED_EDGE ( 'NONE', *, *, #12890, .T. ) ;
#4689 = B_SPLINE_CURVE_WITH_KNOTS ( 'NONE', 3,
 ( #13700, #11535, #4251, #10316 ),
 .UNSPECIFIED., .F., .F.,
 ( 4, 4 ),
 ( 0.005123713096549378093, 0.005814346476695809313 ),
 .UNSPECIFIED. ) ;
#4690 = CARTESIAN_POINT ( 'NONE',  ( 0.000000000000000000, 9.324097380959777581, -22.25075486061729535 ) ) ;
#4691 = CARTESIAN_POINT ( 'NONE',  ( 60.23740434540291488, 32.40236306526279009, 5.000000000000000888 ) ) ;
#4692 = LINE ( 'NONE', #2593, #10492 ) ;
#4693 = CARTESIAN_POINT ( 'NONE',  ( 0.000000000000000000, 0.000000000000000000, 0.000000000000000000 ) ) ;
#4694 = DIRECTION ( 'NONE',  ( 0.000000000000000000, 0.000000000000000000, 1.000000000000000000 ) ) ;
#4695 = EDGE_CURVE ( 'NONE', #9070, #3664, #4058, .T. ) ;
#4696 = FACE_OUTER_BOUND ( 'NONE', #10904, .T. ) ;
#4697 = PLANE ( 'NONE',  #11504 ) ;
#4698 = EDGE_CURVE ( 'NONE', #10310, #952, #6283, .T. ) ;
#4699 = ADVANCED_FACE ( 'NONE', ( #1678 ), #7521, .T. ) ;
#4700 = ORIENTED_EDGE ( 'NONE', *, *, #1134, .F. ) ;
#4701 = DIRECTION ( 'NONE',  ( 1.000000000000000000, 0.000000000000000000, 0.000000000000000000 ) ) ;
#4702 = CARTESIAN_POINT ( 'NONE',  ( 0.8958345380406140812, -24.59696699259434993, 12.96989951879399250 ) ) ;
#4703 = VERTEX_POINT ( 'NONE', #6362 ) ;
#4704 = VERTEX_POINT ( 'NONE', #12110 ) ;
#4705 = VERTEX_POINT ( 'NONE', #9660 ) ;
#4706 = ORIENTED_EDGE ( 'NONE', *, *, #6521, .F. ) ;
#4707 = DIRECTION ( 'NONE',  ( 0.000000000000000000, 0.000000000000000000, 1.000000000000000000 ) ) ;
#4708 = CARTESIAN_POINT ( 'NONE',  ( 0.4522159317772141973, -5.191253194755903522, -15.84984805378637063 ) ) ;
#4709 = CARTESIAN_POINT ( 'NONE',  ( 1.394999999999999574, -4.633866840648735774, -27.68468304288263582 ) ) ;
#4710 = DIRECTION ( 'NONE',  ( -0.000000000000000000, -0.000000000000000000, -1.000000000000000000 ) ) ;
#4711 = EDGE_CURVE ( 'NONE', #14392, #15110, #275, .T. ) ;
#4712 = ADVANCED_FACE ( 'NONE', ( #14359 ), #8588, .F. ) ;
#4713 = CARTESIAN_POINT ( 'NONE',  ( 0.1855657389739082119, 5.253342437939721776, 25.39738473785002881 ) ) ;
#4714 = EDGE_CURVE ( 'NONE', #11238, #2991, #1361, .T. ) ;
#4715 = ORIENTED_EDGE ( 'NONE', *, *, #9653, .T. ) ;
#4716 = CARTESIAN_POINT ( 'NONE',  ( 56.98919079003883326, 3.953582723775848962, 2.999999999999999112 ) ) ;
#4717 = EDGE_CURVE ( 'NONE', #5935, #14375, #1021, .T. ) ;
#4718 = ORIENTED_EDGE ( 'NONE', *, *, #4776, .T. ) ;
#4719 = DIRECTION ( 'NONE',  ( 0.000000000000000000, 0.000000000000000000, 1.000000000000000000 ) ) ;
#4720 = PLANE ( 'NONE',  #9221 ) ;
#4721 = EDGE_LOOP ( 'NONE', ( #13299, #1651, #10822, #9368 ) ) ;
#4722 = ORIENTED_EDGE ( 'NONE', *, *, #8548, .F. ) ;
#4723 = FACE_OUTER_BOUND ( 'NONE', #3914, .T. ) ;
#4724 = ORIENTED_EDGE ( 'NONE', *, *, #942, .F. ) ;
#4725 = VECTOR ( 'NONE', #6743, 1000.000000000000114 ) ;
#4726 = CARTESIAN_POINT ( 'NONE',  ( 1.039999999999994929, -25.12109765559662833, 12.52377138324214023 ) ) ;
#4727 = DIRECTION ( 'NONE',  ( 1.000000000000000000, 0.000000000000000000, 0.000000000000000000 ) ) ;
#4728 = CARTESIAN_POINT ( 'NONE',  ( 2.790000000000079527, 18.34439787333507255, 15.96555658743769079 ) ) ;
#4729 = CARTESIAN_POINT ( 'NONE',  ( 84.00000000000000000, 0.000000000000000000, -131.1575142076926852 ) ) ;
#4730 = ORIENTED_EDGE ( 'NONE', *, *, #8613, .T. ) ;
#4731 = DIRECTION ( 'NONE',  ( -0.000000000000000000, -0.000000000000000000, -1.000000000000000000 ) ) ;
#4732 = B_SPLINE_CURVE_WITH_KNOTS ( 'NONE', 3,
 ( #2138, #10135, #10288, #14907 ),
 .UNSPECIFIED., .F., .F.,
 ( 4, 4 ),
 ( 2.034713381942717888E-07, 0.0006887909409525252036 ),
 .UNSPECIFIED. ) ;
#4733 = CARTESIAN_POINT ( 'NONE',  ( 2.789999999999999147, 14.55412442567617681, 19.64056340710880022 ) ) ;
#4734 = ORIENTED_EDGE ( 'NONE', *, *, #4250, .T. ) ;
#4735 = VECTOR ( 'NONE', #5693, 1000.000000000000000 ) ;
#4736 = ORIENTED_EDGE ( 'NONE', *, *, #14171, .F. ) ;
#4737 = DIRECTION ( 'NONE',  ( -0.000000000000000000, -0.000000000000000000, 1.000000000000000000 ) ) ;
#4738 = CARTESIAN_POINT ( 'NONE',  ( 2.789999999999999147, 13.87420763704361093, -1.948757464274220697 ) ) ;
#4739 = CARTESIAN_POINT ( 'NONE',  ( 2.764680872515352217, 14.46287784598617243, 2.311161484776605324 ) ) ;
#4740 = CARTESIAN_POINT ( 'NONE',  ( 98.33955663538051795, 3.898681236723621879, 2.999999999999999112 ) ) ;
#4741 = DIRECTION ( 'NONE',  ( 1.000000000000000000, 0.000000000000000000, 0.000000000000000000 ) ) ;
#4742 = EDGE_CURVE ( 'NONE', #4311, #14060, #15049, .T. ) ;
#4743 = CARTESIAN_POINT ( 'NONE',  ( -1.150000000000000577, 0.000000000000000000, 0.000000000000000000 ) ) ;
#4744 = ORIENTED_EDGE ( 'NONE', *, *, #12577, .F. ) ;
#4745 = CARTESIAN_POINT ( 'NONE',  ( 2.789999999999999147, -13.68080036884352246, 5.229914364928304416 ) ) ;
#4746 = CARTESIAN_POINT ( 'NONE',  ( 80.00000000000000000, 0.000000000000000000, 4.500000000000000888 ) ) ;
#4747 = CARTESIAN_POINT ( 'NONE',  ( 2.789999999999999147, 15.04425356660760293, 20.70663861606276868 ) ) ;
#4748 = CARTESIAN_POINT ( 'NONE',  ( 2.789999999999999147, 0.000000000000000000, 0.000000000000000000 ) ) ;
#4749 = AXIS2_PLACEMENT_3D ( 'NONE', #4206, #14881, #739 ) ;
#4750 = EDGE_LOOP ( 'NONE', ( #3769, #8499, #7695, #9815 ) ) ;
#4751 = EDGE_LOOP ( 'NONE', ( #1213, #6500, #11107, #7625, #14080, #14774, #3834, #14011 ) ) ;
#4752 = CARTESIAN_POINT ( 'NONE',  ( 0.5279273381794625797, 26.82026385750178932, 3.461047254864356049 ) ) ;
#4753 = ORIENTED_EDGE ( 'NONE', *, *, #5177, .T. ) ;
#4754 = CYLINDRICAL_SURFACE ( 'NONE', #9018, 2.524999999999996358 ) ;
#4755 = CARTESIAN_POINT ( 'NONE',  ( 1.566204647097437341, -6.822536405429464601, -0.8000000000000000444 ) ) ;
#4756 = CARTESIAN_POINT ( 'NONE',  ( 0.1085714285714285687, -3.798448662927795372, 0.000000000000000000 ) ) ;
#4757 = LINE ( 'NONE', #4920, #9449 ) ;
#4758 = DIRECTION ( 'NONE',  ( -1.000000000000000000, -0.000000000000000000, -0.000000000000000000 ) ) ;
#4759 = B_SPLINE_CURVE_WITH_KNOTS ( 'NONE', 3,
 ( #4442, #9124, #11568, #11343, #3138, #1046 ),
 .UNSPECIFIED., .F., .F.,
 ( 4, 2, 4 ),
 ( 4.462636682233640623E-07, 0.001879885020955585333, 0.003759323778242947261 ),
 .UNSPECIFIED. ) ;
#4760 = DIRECTION ( 'NONE',  ( 0.000000000000000000, 0.000000000000000000, 1.000000000000000000 ) ) ;
#4761 = CARTESIAN_POINT ( 'NONE',  ( 101.4858053992934401, 0.9022481406819604643, 2.999999999999999112 ) ) ;
#4762 = AXIS2_PLACEMENT_3D ( 'NONE', #7442, #12109, #10662 ) ;
#4763 = ORIENTED_EDGE ( 'NONE', *, *, #7486, .F. ) ;
#4764 = DIRECTION ( 'NONE',  ( 0.000000000000000000, -1.224646799147353207E-16, 1.000000000000000000 ) ) ;
#4765 = CARTESIAN_POINT ( 'NONE',  ( 1.749999999999998002, -27.76164181293054511, 4.147968289691195132 ) ) ;
#4766 = ADVANCED_FACE ( 'NONE', ( #5154 ), #14519, .F. ) ;
#4767 =( LENGTH_UNIT ( ) NAMED_UNIT ( * ) SI_UNIT ( .MILLI., .METRE. ) );
#4768 = EDGE_LOOP ( 'NONE', ( #8741, #14497, #9548, #6568 ) ) ;
#4769 = B_SPLINE_CURVE_WITH_KNOTS ( 'NONE', 3,
 ( #14025, #2346, #3493, #8181, #1197, #2426, #5891, #10573 ),
 .UNSPECIFIED., .F., .F.,
 ( 4, 2, 2, 4 ),
 ( 4.663089341996299912E-07, 0.001898630032275737097, 0.002847711893946505961, 0.003796793755617274609 ),
 .UNSPECIFIED. ) ;
#4770 = FILL_AREA_STYLE_COLOUR ( '', #5340 ) ;
#4771 = CIRCLE ( 'NONE', #8676, 4.872650870659752442 ) ;
#4772 = ORIENTED_EDGE ( 'NONE', *, *, #5346, .T. ) ;
#4773 = ORIENTED_EDGE ( 'NONE', *, *, #8992, .F. ) ;
#4774 = ORIENTED_EDGE ( 'NONE', *, *, #8675, .T. ) ;
#4775 = FACE_OUTER_BOUND ( 'NONE', #2110, .T. ) ;
#4776 = EDGE_CURVE ( 'NONE', #9529, #3101, #890, .T. ) ;
#4777 = CARTESIAN_POINT ( 'NONE',  ( 8.000000000000000000, 0.000000000000000000, 0.000000000000000000 ) ) ;
#4778 = EDGE_CURVE ( 'NONE', #5632, #11410, #268, .T. ) ;
#4779 = EDGE_CURVE ( 'NONE', #2934, #7330, #3034, .T. ) ;
#4780 = FACE_OUTER_BOUND ( 'NONE', #9358, .T. ) ;
#4781 = CARTESIAN_POINT ( 'NONE',  ( -14.40394475573011945, -10.79473832354794283, -3.799999999999999822 ) ) ;
#4782 = AXIS2_PLACEMENT_3D ( 'NONE', #8833, #5400, #6305 ) ;
#4783 = VECTOR ( 'NONE', #7484, 1000.000000000000000 ) ;
#4785 = CIRCLE ( 'NONE', #12617, 4.424999999999999822 ) ;
#4784 = CARTESIAN_POINT ( 'NONE',  ( 0.07186815222487989707, 5.344160105508701797, 24.78765742476140943 ) ) ;
#4786 = VERTEX_POINT ( 'NONE', #12510 ) ;
#4787 = DIRECTION ( 'NONE',  ( -1.000000000000000000, 0.000000000000000000, 0.000000000000000000 ) ) ;
#4788 = EDGE_CURVE ( 'NONE', #3473, #1894, #13974, .T. ) ;
#4789 = AXIS2_PLACEMENT_3D ( 'NONE', #14280, #10661, #9514 ) ;
#4790 = ADVANCED_FACE ( 'NONE', ( #10198 ), #1822, .F. ) ;
#4791 = TOROIDAL_SURFACE ( 'NONE', #10668, 24.12539914357697413, 8.000000000000000000 ) ;
#4792 = CIRCLE ( 'NONE', #13099, 4.424999999999999822 ) ;
#4793 = ORIENTED_EDGE ( 'NONE', *, *, #4587, .T. ) ;
#4794 = CARTESIAN_POINT ( 'NONE',  ( 2.765633920072238627, -21.30679549418621832, -12.59161484032935618 ) ) ;
#4795 = CARTESIAN_POINT ( 'NONE',  ( 8.000000000000000000, 0.000000000000000000, 0.000000000000000000 ) ) ;
#4796 = EDGE_CURVE ( 'NONE', #3644, #5314, #8884, .T. ) ;
#4797 = ORIENTED_EDGE ( 'NONE', *, *, #12293, .T. ) ;
#4798 = VERTEX_POINT ( 'NONE', #13508 ) ;
#4799 = ORIENTED_EDGE ( 'NONE', *, *, #7701, .T. ) ;
#4800 = CARTESIAN_POINT ( 'NONE',  ( 2.789999999999999147, -22.25075486061731667, -9.324097380959683434 ) ) ;
#4801 = CIRCLE ( 'NONE', #3322, 24.12539914357697768 ) ;
#4802 = EDGE_CURVE ( 'NONE', #8896, #228, #3178, .T. ) ;
#4803 = VERTEX_POINT ( 'NONE', #3139 ) ;
#4804 = AXIS2_PLACEMENT_3D ( 'NONE', #6467, #12381, #1863 ) ;
#4805 = CARTESIAN_POINT ( 'NONE',  ( 75.68384697807671557, 11.35494834827056110, 2.999999999999999112 ) ) ;
#4806 = CARTESIAN_POINT ( 'NONE',  ( 1.394999999999999574, 4.147968289691677413, -27.76164181293047761 ) ) ;
#4807 = CARTESIAN_POINT ( 'NONE',  ( 1.394999999999998685, -4.458161950358380921, -17.39253030560846369 ) ) ;
#4808 = DIRECTION ( 'NONE',  ( 0.000000000000000000, 0.000000000000000000, -1.000000000000000000 ) ) ;
#4809 = ORIENTED_EDGE ( 'NONE', *, *, #622, .F. ) ;
#4810 = CARTESIAN_POINT ( 'NONE',  ( 14.40394475573011945, -10.79473832354794460, 22.47056274847713908 ) ) ;
#4811 = LINE ( 'NONE', #9483, #5342 ) ;
#4812 = ORIENTED_EDGE ( 'NONE', *, *, #936, .T. ) ;
#4813 = VERTEX_POINT ( 'NONE', #11346 ) ;
#4814 = CARTESIAN_POINT ( 'NONE',  ( 0.02531912748679520167, -11.36963888406680923, -9.232963481057881339 ) ) ;
#4815 = CARTESIAN_POINT ( 'NONE',  ( -17.83201772771817772, -12.43434672152745613, -2.999999999999999556 ) ) ;
#4816 = DIRECTION ( 'NONE',  ( -1.000000000000000000, -0.000000000000000000, -0.000000000000000000 ) ) ;
#4817 = LINE ( 'NONE', #14188, #8462 ) ;
#4818 = LINE ( 'NONE', #5341, #209 ) ;
#4819 = PRODUCT_DEFINITION_SHAPE ( 'NONE', 'NONE',  #3450 ) ;
#4820 = CARTESIAN_POINT ( 'NONE',  ( 2.031033471609898111, -27.31260702007178409, 3.797536611356223890 ) ) ;
#4821 = AXIS2_PLACEMENT_3D ( 'NONE', #15098, #1405, #12775 ) ;
#4822 = EDGE_LOOP ( 'NONE', ( #11425, #3597, #7785, #3476 ) ) ;
#4823 = DIRECTION ( 'NONE',  ( 0.000000000000000000, 0.000000000000000000, 1.000000000000000000 ) ) ;
#4824 = DIRECTION ( 'NONE',  ( 1.000000000000000000, 0.000000000000000000, 0.000000000000000000 ) ) ;
#4825 = DIRECTION ( 'NONE',  ( 0.000000000000000000, 0.000000000000000000, -1.000000000000000000 ) ) ;
#4826 = CARTESIAN_POINT ( 'NONE',  ( 2.783025228907522575, 22.53337530003403799, 9.686319561461028016 ) ) ;
#4827 = ORIENTED_EDGE ( 'NONE', *, *, #2811, .F. ) ;
#4828 = ORIENTED_EDGE ( 'NONE', *, *, #10773, .F. ) ;
#4829 = VECTOR ( 'NONE', #1229, 1000.000000000000000 ) ;
#4830 = ORIENTED_EDGE ( 'NONE', *, *, #6135, .T. ) ;
#4831 = DIRECTION ( 'NONE',  ( -1.000000000000000000, -0.000000000000000000, -0.000000000000000000 ) ) ;
#4832 = AXIS2_PLACEMENT_3D ( 'NONE', #4608, #175, #2565 ) ;
#4833 = CARTESIAN_POINT ( 'NONE',  ( 0.02436607992776585255, -5.391175441198789109, 24.15498966839961170 ) ) ;
#4834 = DIRECTION ( 'NONE',  ( -1.000000000000000000, -0.000000000000000000, -0.000000000000000000 ) ) ;
#4835 = AXIS2_PLACEMENT_3D ( 'NONE', #11018, #7489, #1493 ) ;
#4836 = DIRECTION ( 'NONE',  ( 0.000000000000000000, 1.000000000000000000, 0.000000000000000000 ) ) ;
#4837 = CARTESIAN_POINT ( 'NONE',  ( 80.00000000000001421, 1.084202172485504434E-16, -5.395000000000002238 ) ) ;
#4838 = CARTESIAN_POINT ( 'NONE',  ( 2.790000000000077307, 20.65026423218591844, -12.51972477286559027 ) ) ;
#4839 = ORIENTED_EDGE ( 'NONE', *, *, #8625, .F. ) ;
#4840 = LINE ( 'NONE', #13984, #5422 ) ;
#4841 = FACE_OUTER_BOUND ( 'NONE', #2732, .T. ) ;
#4842 = ORIENTED_EDGE ( 'NONE', *, *, #3509, .F. ) ;
#4844 = AXIS2_PLACEMENT_3D ( 'NONE', #12797, #12871, #2285 ) ;
#4843 = CARTESIAN_POINT ( 'NONE',  ( -0.1085714285714285687, -3.798448662927795372, -0.8000000000000000444 ) ) ;
#4845 = CARTESIAN_POINT ( 'NONE',  ( 2.563317066925346527E-16, -12.51294990530000817, -20.85230829256867935 ) ) ;
#4846 = DIRECTION ( 'NONE',  ( 0.000000000000000000, 0.000000000000000000, 1.000000000000000000 ) ) ;
#4847 = ADVANCED_FACE ( 'NONE', ( #5450 ), #4659, .T. ) ;
#4848 = ORIENTED_EDGE ( 'NONE', *, *, #4177, .F. ) ;
#4849 = AXIS2_PLACEMENT_3D ( 'NONE', #8901, #4458, #10211 ) ;
#4850 = CIRCLE ( 'NONE', #1904, 28.06981291497571007 ) ;
#4851 = ADVANCED_FACE ( 'NONE', ( #6432 ), #8816, .F. ) ;
#4852 = AXIS2_PLACEMENT_3D ( 'NONE', #11676, #10609, #1237 ) ;
#4853 = ORIENTED_EDGE ( 'NONE', *, *, #1214, .F. ) ;
#4854 = ORIENTED_EDGE ( 'NONE', *, *, #12731, .T. ) ;
#4855 = ORIENTED_EDGE ( 'NONE', *, *, #8911, .T. ) ;
#4856 = CARTESIAN_POINT ( 'NONE',  ( 1.039999999999997593, 0.000000000000000000, 0.000000000000000000 ) ) ;
#4857 = CARTESIAN_POINT ( 'NONE',  ( 1.387778780781445676E-14, 0.000000000000000000, -7.800000000000008704 ) ) ;
#4858 = AXIS2_PLACEMENT_3D ( 'NONE', #4810, #2339, #10634 ) ;
#4859 = EDGE_CURVE ( 'NONE', #2773, #14197, #831, .T. ) ;
#4860 = CARTESIAN_POINT ( 'NONE',  ( 2.764680872515351329, 14.46287784598617421, -2.311161484776606212 ) ) ;
#4861 = CARTESIAN_POINT ( 'NONE',  ( 0.000000000000000000, -15.74360496233395956, 18.28042085475273026 ) ) ;
#4862 = AXIS2_PLACEMENT_3D ( 'NONE', #10046, #14743, #9121 ) ;
#4863 = CARTESIAN_POINT ( 'NONE',  ( 2.582362745529150683, 12.04200105039470259, 10.30022894898810293 ) ) ;
#4864 = VERTEX_POINT ( 'NONE', #4214 ) ;
#4865 = DIRECTION ( 'NONE',  ( 0.000000000000000000, 0.000000000000000000, 1.000000000000000000 ) ) ;
#4866 = AXIS2_PLACEMENT_3D ( 'NONE', #7380, #13514, #1523 ) ;
#4867 = EDGE_CURVE ( 'NONE', #9019, #5489, #13232, .T. ) ;
#4868 = EDGE_CURVE ( 'NONE', #5535, #7552, #15217, .T. ) ;
#4869 = CIRCLE ( 'NONE', #3398, 24.12539914357697768 ) ;
#4870 = B_SPLINE_CURVE_WITH_KNOTS ( 'NONE', 3,
 ( #6023, #6104, #8469, #2935, #7340, #12006 ),
 .UNSPECIFIED., .F., .F.,
 ( 4, 2, 4 ),
 ( 1.979325885387340151E-07, 0.001878588715165610589, 0.003756979497742682708 ),
 .UNSPECIFIED. ) ;
#4871 = ORIENTED_EDGE ( 'NONE', *, *, #6559, .T. ) ;
#4872 = CARTESIAN_POINT ( 'NONE',  ( 86.17559721729969624, 12.01344854909570259, 2.999999999999999112 ) ) ;
#4873 = CARTESIAN_POINT ( 'NONE',  ( 0.09203968221122160731, -14.31435947614538406, -5.280991956247265584 ) ) ;
#4874 = ORIENTED_EDGE ( 'NONE', *, *, #1394, .F. ) ;
#4875 = ORIENTED_EDGE ( 'NONE', *, *, #11530, .F. ) ;
#4876 = CIRCLE ( 'NONE', #7321, 0.5999999999999998668 ) ;
#4877 = AXIS2_PLACEMENT_3D ( 'NONE', #7801, #14726, #643 ) ;
#4878 = CARTESIAN_POINT ( 'NONE',  ( 0.000000000000000000, 0.000000000000000000, 0.000000000000000000 ) ) ;
#4879 = EDGE_CURVE ( 'NONE', #2234, #7890, #5149, .T. ) ;
#4880 = ORIENTED_EDGE ( 'NONE', *, *, #11693, .T. ) ;
#4881 = DIRECTION ( 'NONE',  ( -1.000000000000000000, 0.000000000000000000, 0.000000000000000000 ) ) ;
#4882 = DIRECTION ( 'NONE',  ( 0.000000000000000000, 0.9510565162951567508, -0.3090169943749379589 ) ) ;
#4883 = EDGE_CURVE ( 'NONE', #7008, #4813, #10547, .T. ) ;
#4884 = EDGE_CURVE ( 'NONE', #8456, #12081, #12575, .T. ) ;
#4885 = CARTESIAN_POINT ( 'NONE',  ( 3.321103546710217014, -13.95673088054953581, 6.000000000000000000 ) ) ;
#4886 = DIRECTION ( 'NONE',  ( 0.000000000000000000, 0.000000000000000000, -1.000000000000000000 ) ) ;
#4887 = AXIS2_PLACEMENT_3D ( 'NONE', #6570, #11172, #10462 ) ;
#4888 = ORIENTED_EDGE ( 'NONE', *, *, #12204, .T. ) ;
#4889 = TOROIDAL_SURFACE ( 'NONE', #12720, 14.01039946648074341, 8.000000000000000000 ) ;
#4890 = CYLINDRICAL_SURFACE ( 'NONE', #805, 4.000000000000000000 ) ;
#4891 = FACE_OUTER_BOUND ( 'NONE', #6013, .T. ) ;
#4892 = ORIENTED_EDGE ( 'NONE', *, *, #7393, .T. ) ;
#4893 = CARTESIAN_POINT ( 'NONE',  ( -9.403944755730119454, -4.794738323547945491, 22.00000000000000000 ) ) ;
#4894 = ADVANCED_FACE ( 'NONE', ( #13427 ), #12942, .F. ) ;
#4895 = ORIENTED_EDGE ( 'NONE', *, *, #4586, .T. ) ;
#4896 = EDGE_LOOP ( 'NONE', ( #14625, #8838 ) ) ;
#4897 = CARTESIAN_POINT ( 'NONE',  ( 2.257825462012207574, 23.74442027961379864, -12.96514671151741638 ) ) ;
#4898 = CARTESIAN_POINT ( 'NONE',  ( 0.006974657972266581039, -23.92335783895634194, -5.408388659524344000 ) ) ;
#4899 = DIRECTION ( 'NONE',  ( 1.000000000000000000, 0.000000000000000000, 0.000000000000000000 ) ) ;
#4900 = APPLICATION_CONTEXT ( 'automotive_design' ) ;
#4901 = DIRECTION ( 'NONE',  ( -1.000000000000000000, 0.000000000000000000, 0.000000000000000000 ) ) ;
#4902 = AXIS2_PLACEMENT_3D ( 'NONE', #10449, #1069, #14051 ) ;
#4904 = CIRCLE ( 'NONE', #10047, 6.000000000000001776 ) ;
#4903 = CARTESIAN_POINT ( 'NONE',  ( -1.093979827056220885E-14, -2.096460570596271111, 14.05347802000168400 ) ) ;
#4905 = FACE_OUTER_BOUND ( 'NONE', #245, .T. ) ;
#4906 = ORIENTED_EDGE ( 'NONE', *, *, #1101, .F. ) ;
#4907 = DIRECTION ( 'NONE',  ( 1.000000000000000000, 0.000000000000000000, 0.000000000000000000 ) ) ;
#4908 = DIRECTION ( 'NONE',  ( 0.000000000000000000, 0.000000000000000000, 1.000000000000000000 ) ) ;
#4909 = DIRECTION ( 'NONE',  ( -1.000000000000000000, -0.000000000000000000, -0.000000000000000000 ) ) ;
#4910 = DIRECTION ( 'NONE',  ( 0.000000000000000000, 0.000000000000000000, -1.000000000000000000 ) ) ;
#4911 = ORIENTED_EDGE ( 'NONE', *, *, #2378, .F. ) ;
#4912 = ADVANCED_BREP_SHAPE_REPRESENTATION ( '', ( #13940, #1376 ), #9175 ) ;
#4913 = CIRCLE ( 'NONE', #3918, 4.999999999999999112 ) ;
#4914 = ORIENTED_EDGE ( 'NONE', *, *, #5548, .T. ) ;
#4915 = EDGE_CURVE ( 'NONE', #1577, #8659, #5960, .T. ) ;
#4916 = ORIENTED_EDGE ( 'NONE', *, *, #3135, .F. ) ;
#4917 = CARTESIAN_POINT ( 'NONE',  ( 2.765633920072234631, -21.30679549418640306, 12.59161484032904887 ) ) ;
#4918 = CARTESIAN_POINT ( 'NONE',  ( 0.000000000000000000, -5.535312321042921369, 23.48180575137728354 ) ) ;
#4919 = DIRECTION ( 'NONE',  ( -1.000000000000000000, 0.000000000000000000, 0.000000000000000000 ) ) ;
#4920 = CARTESIAN_POINT ( 'NONE',  ( -12.16787677823033142, -4.794738323547945491, 14.99999999999999822 ) ) ;
#4921 = DIRECTION ( 'NONE',  ( -1.000000000000000000, 0.000000000000000000, 0.000000000000000000 ) ) ;
#4922 = ORIENTED_EDGE ( 'NONE', *, *, #1394, .T. ) ;
#4923 = CARTESIAN_POINT ( 'NONE',  ( 0.02436607992775891365, -24.63872515616080960, -2.336989772644527008 ) ) ;
#4924 = LINE ( 'NONE', #13906, #2931 ) ;
#4925 = CIRCLE ( 'NONE', #13500, 6.000000000000000888 ) ;
#4926 = VERTEX_POINT ( 'NONE', #971 ) ;
#4927 = LINE ( 'NONE', #9596, #14190 ) ;
#4928 = CARTESIAN_POINT ( 'NONE',  ( 0.1920562174424401414, 10.28947301956298865, -12.05486625177560711 ) ) ;
#4929 = LINE ( 'NONE', #12974, #348 ) ;
#4930 = EDGE_CURVE ( 'NONE', #6544, #7716, #6119, .T. ) ;
#4931 = ORIENTED_EDGE ( 'NONE', *, *, #7955, .F. ) ;
#4932 = PRESENTATION_STYLE_ASSIGNMENT (( #5988 ) ) ;
#4933 = VERTEX_POINT ( 'NONE', #8185 ) ;
#4934 = ORIENTED_EDGE ( 'NONE', *, *, #11047, .T. ) ;
#4935 = ORIENTED_EDGE ( 'NONE', *, *, #2070, .T. ) ;
#4936 = FACE_BOUND ( 'NONE', #2713, .T. ) ;
#4937 = CARTESIAN_POINT ( 'NONE',  ( 2.790000000000076863, -23.69897269326681055, 5.456611084821764379 ) ) ;
#4938 = PLANE ( 'NONE',  #10993 ) ;
#4939 = CARTESIAN_POINT ( 'NONE',  ( 93.34550147531103903, 3.654933296868752457, 7.000000000000000000 ) ) ;
#4940 = CARTESIAN_POINT ( 'NONE',  ( 0.000000000000000000, 22.25075486061737351, 9.324097380959511128 ) ) ;
#4941 = EDGE_CURVE ( 'NONE', #9696, #4314, #459, .T. ) ;
#4942 = CYLINDRICAL_SURFACE ( 'NONE', #1709, 2.000000000000000444 ) ;
#4943 = EDGE_CURVE ( 'NONE', #11143, #9391, #6880, .T. ) ;
#4944 = ORIENTED_EDGE ( 'NONE', *, *, #10881, .F. ) ;
#4945 = DIRECTION ( 'NONE',  ( 0.4571871344001384174, 0.8893705212896307888, -0.000000000000000000 ) ) ;
#4946 = ORIENTED_EDGE ( 'NONE', *, *, #2915, .F. ) ;
#4947 = DIRECTION ( 'NONE',  ( 0.000000000000000000, 0.000000000000000000, 1.000000000000000000 ) ) ;
#4948 = DIRECTION ( 'NONE',  ( 0.000000000000000000, 0.000000000000000000, 1.000000000000000000 ) ) ;
#4949 = ORIENTED_EDGE ( 'NONE', *, *, #1846, .F. ) ;
#4950 = ORIENTED_EDGE ( 'NONE', *, *, #10916, .F. ) ;
#4951 = FACE_OUTER_BOUND ( 'NONE', #5911, .T. ) ;
#4952 = ORIENTED_EDGE ( 'NONE', *, *, #7230, .T. ) ;
#4953 = CARTESIAN_POINT ( 'NONE',  ( 2.789999999999999147, 12.59161484032912171, 21.30679549418635688 ) ) ;
#4954 = CARTESIAN_POINT ( 'NONE',  ( 4.000000000000000888, 4.898587196589413815E-16, -10.00000000000000000 ) ) ;
#4955 = VECTOR ( 'NONE', #718, 1000.000000000000000 ) ;
#4956 = CARTESIAN_POINT ( 'NONE',  ( 111.6227766016837961, 7.610970684806392799E-15, 4.000000000000003553 ) ) ;
#4957 = EDGE_CURVE ( 'NONE', #4704, #1510, #9544, .T. ) ;
#4958 = EDGE_LOOP ( 'NONE', ( #704, #10566, #4164, #441, #12288, #10189, #8080, #996 ) ) ;
#4959 = DIRECTION ( 'NONE',  ( -0.000000000000000000, -0.000000000000000000, 1.000000000000000000 ) ) ;
#4960 = CARTESIAN_POINT ( 'NONE',  ( 67.23404255319148604, 28.93147646537027384, 3.000000000000002665 ) ) ;
#4961 = VERTEX_POINT ( 'NONE', #10422 ) ;
#4962 = DIRECTION ( 'NONE',  ( 1.000000000000000000, 0.000000000000000000, 0.000000000000000000 ) ) ;
#4963 = ORIENTED_EDGE ( 'NONE', *, *, #130, .T. ) ;
#4964 = ORIENTED_EDGE ( 'NONE', *, *, #8428, .F. ) ;
#4965 = SURFACE_SIDE_STYLE ('',( #12253 ) ) ;
#4966 = CARTESIAN_POINT ( 'NONE',  ( 2.765633920072235519, -9.836394144775869819, 22.71065055754449347 ) ) ;
#4967 = ADVANCED_FACE ( 'NONE', ( #9126 ), #957, .T. ) ;
#4968 = EDGE_CURVE ( 'NONE', #3623, #9188, #9199, .T. ) ;
#4969 = VECTOR ( 'NONE', #337, 1000.000000000000000 ) ;
#4970 =( NAMED_UNIT ( * ) SI_UNIT ( $, .STERADIAN. ) SOLID_ANGLE_UNIT ( ) );
#4971 = DIRECTION ( 'NONE',  ( 1.445602896647338917E-16, -1.000000000000000000, 0.000000000000000000 ) ) ;
#4972 = CARTESIAN_POINT ( 'NONE',  ( 2.789999999999999147, -18.55949924794904504, 16.37294372382852004 ) ) ;
#4973 = CARTESIAN_POINT ( 'NONE',  ( 8.000000000000000000, 0.000000000000000000, 0.000000000000000000 ) ) ;
#4974 = ORIENTED_EDGE ( 'NONE', *, *, #540, .F. ) ;
#4975 = DIRECTION ( 'NONE',  ( -0.4036950204470267645, 0.9148936170212768060, 0.000000000000000000 ) ) ;
#4976 = CARTESIAN_POINT ( 'NONE',  ( 1.749999999999999778, 0.000000000000000000, 0.000000000000000000 ) ) ;
#4977 = CARTESIAN_POINT ( 'NONE',  ( 2.236220346785029012, -3.624349476775082124, -16.55730827443884934 ) ) ;
#4978 = LINE ( 'NONE', #9648, #9257 ) ;
#4979 = AXIS2_PLACEMENT_3D ( 'NONE', #11741, #12965, #2454 ) ;
#4980 = AXIS2_PLACEMENT_3D ( 'NONE', #7361, #1661, #11033 ) ;
#4981 = ORIENTED_EDGE ( 'NONE', *, *, #15215, .T. ) ;
#4982 = ADVANCED_FACE ( 'NONE', ( #13880 ), #2351, .F. ) ;
#4983 = ORIENTED_EDGE ( 'NONE', *, *, #823, .F. ) ;
#4984 = EDGE_CURVE ( 'NONE', #1778, #2051, #4904, .T. ) ;
#4985 = B_SPLINE_CURVE_WITH_KNOTS ( 'NONE', 3,
 ( #2734, #557, #7423, #12089, #11025, #10867 ),
 .UNSPECIFIED., .F., .F.,
 ( 4, 2, 4 ),
 ( 2.586195665736120714E-07, 0.001878649493629690539, 0.003757040367692807744 ),
 .UNSPECIFIED. ) ;
#4986 = ORIENTED_EDGE ( 'NONE', *, *, #9304, .F. ) ;
#4987 = APPLICATION_CONTEXT ( 'automotive_design' ) ;
#4988 = DIRECTION ( 'NONE',  ( -1.000000000000000000, -0.000000000000000000, -0.000000000000000000 ) ) ;
#4989 = DIRECTION ( 'NONE',  ( -0.4036950204470279302, 0.9148936170212763619, 1.734723475976804333E-15 ) ) ;
#4990 = EDGE_CURVE ( 'NONE', #9577, #3479, #5897, .T. ) ;
#4991 = DIRECTION ( 'NONE',  ( -0.4036950204470267645, 0.9148936170212768060, 0.000000000000000000 ) ) ;
#4992 = CARTESIAN_POINT ( 'NONE',  ( 0.07186815222488067423, -24.78765742476142719, 5.344160105508607650 ) ) ;
#4993 = DIRECTION ( 'NONE',  ( -0.1473126338456099416, 0.9890899796830767698, 0.000000000000000000 ) ) ;
#4994 = CARTESIAN_POINT ( 'NONE',  ( 8.403944755730119454, -10.79473832354794460, 3.000000000000000000 ) ) ;
#4995 = AXIS2_PLACEMENT_3D ( 'NONE', #8110, #12782, #1258 ) ;
#4996 = ORIENTED_EDGE ( 'NONE', *, *, #5458, .T. ) ;
#4997 = DIRECTION ( 'NONE',  ( 1.000000000000000000, 0.000000000000000000, 0.000000000000000000 ) ) ;
#4998 = CARTESIAN_POINT ( 'NONE',  ( 2.790000000000077751, 12.51293083811798645, 20.85287692521934488 ) ) ;
#4999 = EDGE_CURVE ( 'NONE', #11073, #6713, #9062, .T. ) ;
#5000 = ORIENTED_EDGE ( 'NONE', *, *, #11497, .F. ) ;
#5001 = DIRECTION ( 'NONE',  ( -0.000000000000000000, -0.000000000000000000, -1.000000000000000000 ) ) ;
#5002 = CARTESIAN_POINT ( 'NONE',  ( 2.601776091974071115, 25.40949241676360515, -5.251266773802107934 ) ) ;
#5003 = CARTESIAN_POINT ( 'NONE',  ( 0.4472135954999577612, 0.000000000000000000, 0.000000000000000000 ) ) ;
#5004 = ORIENTED_EDGE ( 'NONE', *, *, #11492, .F. ) ;
#5005 = LINE ( 'NONE', #14457, #14893 ) ;
#5006 = DIRECTION ( 'NONE',  ( -1.000000000000000000, 0.000000000000000000, -0.000000000000000000 ) ) ;
#5007 = VERTEX_POINT ( 'NONE', #4512 ) ;
#5008 = ORIENTED_EDGE ( 'NONE', *, *, #8213, .F. ) ;
#5009 = VERTEX_POINT ( 'NONE', #3354 ) ;
#5010 = CARTESIAN_POINT ( 'NONE',  ( 1.249999999999997558, 5.419062086227038392E-16, 4.424999999999999822 ) ) ;
#5011 = CARTESIAN_POINT ( 'NONE',  ( 2.262072769566602304, 11.57956866523218586, 24.43806413951680767 ) ) ;
#5012 = CARTESIAN_POINT ( 'NONE',  ( 0.9041604829517133624, 17.20101185194000593, 4.239993951493269186 ) ) ;
#5013 = CARTESIAN_POINT ( 'NONE',  ( 1.394999999999998685, 19.67366047555559661, -20.02152543075324331 ) ) ;
#5014 = CARTESIAN_POINT ( 'NONE',  ( 1.006169830977205581, -4.228366069762346413, 6.000000000000000000 ) ) ;
#5015 = FACE_OUTER_BOUND ( 'NONE', #4473, .T. ) ;
#5016 = VERTEX_POINT ( 'NONE', #9347 ) ;
#5017 = B_SPLINE_CURVE_WITH_KNOTS ( 'NONE', 3,
 ( #5347, #10015, #6326, #11011, #6402, #474 ),
 .UNSPECIFIED., .F., .F.,
 ( 4, 2, 4 ),
 ( 4.462636731830560059E-07, 0.001879885066974964830, 0.003759323870276746679 ),
 .UNSPECIFIED. ) ;
#5018 = CARTESIAN_POINT ( 'NONE',  ( -16.96657417111497068, -13.60061260430328467, 0.7999999999999960476 ) ) ;
#5019 = EDGE_CURVE ( 'NONE', #9188, #3101, #8812, .T. ) ;
#5020 =( NAMED_UNIT ( * ) PLANE_ANGLE_UNIT ( ) SI_UNIT ( $, .RADIAN. ) );
#5021 = ORIENTED_EDGE ( 'NONE', *, *, #2329, .F. ) ;
#5022 = ORIENTED_EDGE ( 'NONE', *, *, #13692, .T. ) ;
#5023 = DIRECTION ( 'NONE',  ( 0.5416238976136762417, -0.8406209333187996124, 0.000000000000000000 ) ) ;
#5024 = EDGE_CURVE ( 'NONE', #8726, #8554, #12563, .T. ) ;
#5025 = DIRECTION ( 'NONE',  ( -5.339417856040274462E-17, -1.063174570779084693E-17, 1.000000000000000000 ) ) ;
#5026 = ORIENTED_EDGE ( 'NONE', *, *, #13760, .T. ) ;
#5027 = AXIS2_PLACEMENT_3D ( 'NONE', #1411, #12240, #5035 ) ;
#5028 = VECTOR ( 'NONE', #15152, 1000.000000000000000 ) ;
#5029 = CIRCLE ( 'NONE', #9183, 3.799999999999999378 ) ;
#5030 = CARTESIAN_POINT ( 'NONE',  ( 80.00000000000000000, 0.000000000000000000, -131.1575142076926852 ) ) ;
#5031 = ORIENTED_EDGE ( 'NONE', *, *, #10245, .T. ) ;
#5032 = CYLINDRICAL_SURFACE ( 'NONE', #11394, 2.999999999999988898 ) ;
#5033 = CARTESIAN_POINT ( 'NONE',  ( 2.246812880117043942, -16.57708379306441415, -3.619024283482240811 ) ) ;
#5034 = AXIS2_PLACEMENT_3D ( 'NONE', #6531, #5320, #4160 ) ;
#5035 = DIRECTION ( 'NONE',  ( 1.000000000000000000, 0.000000000000000000, 0.000000000000000000 ) ) ;
#5036 = AXIS2_PLACEMENT_3D ( 'NONE', #6306, #5241, #2702 ) ;
#5037=STYLED_ITEM('',(#15272),#3266);
#5038 = EDGE_LOOP ( 'NONE', ( #7408, #6919 ) ) ;
#5039 = CARTESIAN_POINT ( 'NONE',  ( 1.749999999999998002, 0.000000000000000000, 0.000000000000000000 ) ) ;
#5040 = DIRECTION ( 'NONE',  ( 0.000000000000000000, 0.000000000000000000, 1.000000000000000000 ) ) ;
#5041 = VERTEX_POINT ( 'NONE', #11642 ) ;
#5042 = CARTESIAN_POINT ( 'NONE',  ( 0.02436607992776151574, 24.15498966839970052, -5.391175441198366336 ) ) ;
#5043 = ADVANCED_FACE ( 'NONE', ( #1124 ), #5824, .T. ) ;
#5044 = DIRECTION ( 'NONE',  ( 0.000000000000000000, 0.000000000000000000, 1.000000000000000000 ) ) ;
#5045 = EDGE_LOOP ( 'NONE', ( #758, #13167, #6781, #1244 ) ) ;
#5046 = ORIENTED_EDGE ( 'NONE', *, *, #2378, .T. ) ;
#5047 = DIRECTION ( 'NONE',  ( 0.000000000000000000, 0.000000000000000000, -1.000000000000000000 ) ) ;
#5049 = DIRECTION ( 'NONE',  ( -1.000000000000000000, -0.000000000000000000, -0.000000000000000000 ) ) ;
#5048 = AXIS2_PLACEMENT_3D ( 'NONE', #1595, #5741, #2206 ) ;
#5050 = AXIS2_PLACEMENT_3D ( 'NONE', #13381, #4176, #4090 ) ;
#5051 = ADVANCED_FACE ( 'NONE', ( #4675 ), #12386, .T. ) ;
#5052 = DIRECTION ( 'NONE',  ( -1.000000000000000000, 0.000000000000000000, 0.000000000000000000 ) ) ;
#5053 = CARTESIAN_POINT ( 'NONE',  ( 80.82762530298222714, -9.999999999999994671, 3.000000000000002665 ) ) ;
#5054 = ORIENTED_EDGE ( 'NONE', *, *, #14433, .T. ) ;
#5055 = CARTESIAN_POINT ( 'NONE',  ( 2.764680872513935128, -5.229914364928447412, 13.68080036884346917 ) ) ;
#5056 = FACE_OUTER_BOUND ( 'NONE', #8772, .T. ) ;
#5057 = DIRECTION ( 'NONE',  ( 1.000000000000000000, 0.000000000000000000, 0.000000000000000000 ) ) ;
#5058 = AXIS2_PLACEMENT_3D ( 'NONE', #2485, #3702, #158 ) ;
#5059 = SURFACE_STYLE_FILL_AREA ( #8576 ) ;
#5060 = EDGE_CURVE ( 'NONE', #851, #2099, #7356, .T. ) ;
#5061 = VECTOR ( 'NONE', #4248, 1000.000000000000000 ) ;
#5062 = EDGE_CURVE ( 'NONE', #13370, #15071, #10010, .T. ) ;
#5063 = EDGE_LOOP ( 'NONE', ( #6939, #10922, #14969, #10933 ) ) ;
#5064 = ORIENTED_EDGE ( 'NONE', *, *, #2799, .T. ) ;
#5065 = ORIENTED_EDGE ( 'NONE', *, *, #14949, .F. ) ;
#5066 = DIRECTION ( 'NONE',  ( 0.000000000000000000, 0.000000000000000000, 1.000000000000000000 ) ) ;
#5067 = CARTESIAN_POINT ( 'NONE',  ( 0.006931054464084583991, -2.248820353273142558, 24.42321038836782776 ) ) ;
#5068 = CARTESIAN_POINT ( 'NONE',  ( 2.789999999999999147, 20.70663861606272249, 15.04425356660767932 ) ) ;
#5069 = DIRECTION ( 'NONE',  ( 0.000000000000000000, 0.000000000000000000, 1.000000000000000000 ) ) ;
#5070 = CARTESIAN_POINT ( 'NONE',  ( -2.792396023744425565E-17, 3.453121352791049239E-17, 7.799999999999999822 ) ) ;
#5071 = CARTESIAN_POINT ( 'NONE',  ( 0.9999999999999997780, -6.008326913195983998, 0.000000000000000000 ) ) ;
#5072 = VECTOR ( 'NONE', #12355, 1000.000000000000000 ) ;
#5073 = EDGE_LOOP ( 'NONE', ( #6126, #4086 ) ) ;
#5074 = DIRECTION ( 'NONE',  ( 0.000000000000000000, -1.000000000000000000, 0.000000000000000000 ) ) ;
#5075 = CARTESIAN_POINT ( 'NONE',  ( 1.749999999999998002, 12.96210679857822257, -24.89775460606818669 ) ) ;
#5076 = EDGE_CURVE ( 'NONE', #8949, #3508, #3402, .T. ) ;
#5077 = ORIENTED_EDGE ( 'NONE', *, *, #14900, .T. ) ;
#5078 = CARTESIAN_POINT ( 'NONE',  ( 0.000000000000000000, -22.25075486061732732, -9.324097380959701198 ) ) ;
#5079 = CARTESIAN_POINT ( 'NONE',  ( 0.000000000000000000, 0.000000000000000000, 1.395000000000000462 ) ) ;
#5080 = CARTESIAN_POINT ( 'NONE',  ( -16.80212006966224791, -13.74240776967763900, -3.794707603699265519E-15 ) ) ;
#5081 = EDGE_CURVE ( 'NONE', #12694, #14059, #12022, .T. ) ;
#5082 = AXIS2_PLACEMENT_3D ( 'NONE', #7144, #4626, #2298 ) ;
#5083 = EDGE_LOOP ( 'NONE', ( #13036, #2139, #11933, #13320 ) ) ;
#5084 = APPLICATION_CONTEXT ( 'automotive_design' ) ;
#5085 = CARTESIAN_POINT ( 'NONE',  ( 2.789999999999999147, -5.535312321042889394, 23.48180575137727999 ) ) ;
#5086 = CARTESIAN_POINT ( 'NONE',  ( 1.039999999999997593, 0.000000000000000000, 0.000000000000000000 ) ) ;
#5087 = ORIENTED_EDGE ( 'NONE', *, *, #7030, .F. ) ;
#5088 = ORIENTED_EDGE ( 'NONE', *, *, #9376, .T. ) ;
#5089 = ORIENTED_EDGE ( 'NONE', *, *, #9187, .F. ) ;
#5090 = DIRECTION ( 'NONE',  ( 1.000000000000000000, 0.000000000000000000, 0.000000000000000000 ) ) ;
#5091 = EDGE_CURVE ( 'NONE', #12774, #10832, #6621, .T. ) ;
#5092 = CARTESIAN_POINT ( 'NONE',  ( 2.790000000000061764, 8.842064619038678686, -11.12234047011180849 ) ) ;
#5093 = CARTESIAN_POINT ( 'NONE',  ( 2.715264245299034762, -9.749517823373922809, -11.74839219818098535 ) ) ;
#5094 = CARTESIAN_POINT ( 'NONE',  ( 14.40394475573011945, -10.79473832354794460, 6.000000000000000000 ) ) ;
#5095 = VECTOR ( 'NONE', #9131, 1000.000000000000000 ) ;
#5096 = CIRCLE ( 'NONE', #12908, 14.01039946648073986 ) ;
#5097 = CARTESIAN_POINT ( 'NONE',  ( 1.249999999999997780, 0.000000000000000000, -4.100000000000000533 ) ) ;
#5098 = EDGE_LOOP ( 'NONE', ( #9928, #3739, #14775, #15220 ) ) ;
#5099 = DIRECTION ( 'NONE',  ( 0.4570747303910189796, -0.8894282943767739535, 6.847307257068339928E-17 ) ) ;
#5100 = CIRCLE ( 'NONE', #5586, 4.000000000000000000 ) ;
#5101 = VECTOR ( 'NONE', #12315, 1000.000000000000000 ) ;
#5102 = AXIS2_PLACEMENT_3D ( 'NONE', #7961, #11567, #1901 ) ;
#5103 = FILL_AREA_STYLE ('',( #11072 ) ) ;
#5104 = PRESENTATION_LAYER_ASSIGNMENT (  '', '', ( #7551 ) ) ;
#5105 = ORIENTED_EDGE ( 'NONE', *, *, #297, .T. ) ;
#5106 = ORIENTED_EDGE ( 'NONE', *, *, #10673, .T. ) ;
#5107 = DIRECTION ( 'NONE',  ( 0.000000000000000000, 0.000000000000000000, 1.000000000000000000 ) ) ;
#5108 = CARTESIAN_POINT ( 'NONE',  ( 0.04999671820202237355, -13.99876742897255255, -5.264737421541672013 ) ) ;
#5109 = ORIENTED_EDGE ( 'NONE', *, *, #11056, .T. ) ;
#5110 = CIRCLE ( 'NONE', #6080, 24.12539914357697413 ) ;
#5111 = CIRCLE ( 'NONE', #5849, 4.000000000000000000 ) ;
#5112 = AXIS2_PLACEMENT_3D ( 'NONE', #9450, #1382, #2470 ) ;
#5113 = AXIS2_PLACEMENT_3D ( 'NONE', #7410, #475, #4882 ) ;
#5114 = DIRECTION ( 'NONE',  ( 1.000000000000000000, 0.000000000000000000, 0.000000000000000000 ) ) ;
#5115 = ORIENTED_EDGE ( 'NONE', *, *, #3525, .F. ) ;
#5116 = CARTESIAN_POINT ( 'NONE',  ( 0.1438988480159978933, 14.59528211758547478, 5.279841123860917307 ) ) ;
#5117 = FACE_OUTER_BOUND ( 'NONE', #9066, .T. ) ;
#5118 = LINE ( 'NONE', #6103, #12369 ) ;
#5119 = CIRCLE ( 'NONE', #181, 4.599999999999999645 ) ;
#5120 = PLANE ( 'NONE',  #12335 ) ;
#5121 = EDGE_CURVE ( 'NONE', #241, #4343, #1428, .T. ) ;
#5122 = DIRECTION ( 'NONE',  ( -1.000000000000000000, 0.000000000000000000, -0.000000000000000000 ) ) ;
#5123 = VECTOR ( 'NONE', #3273, 1000.000000000000000 ) ;
#5124 = VECTOR ( 'NONE', #6065, 1000.000000000000000 ) ;
#5125 = VERTEX_POINT ( 'NONE', #6469 ) ;
#5126 = CARTESIAN_POINT ( 'NONE',  ( 0.000000000000000000, 0.000000000000000000, 3.895000000000000462 ) ) ;
#5127 = DIRECTION ( 'NONE',  ( -1.000000000000000000, 0.000000000000000000, 0.000000000000000000 ) ) ;
#5128 = ORIENTED_EDGE ( 'NONE', *, *, #629, .T. ) ;
#5129 = EDGE_LOOP ( 'NONE', ( #4270, #9964, #15197, #4403 ) ) ;
#5130 = CARTESIAN_POINT ( 'NONE',  ( 2.765633920072235963, -16.37294372382871188, 18.55949924794887096 ) ) ;
#5131 = SURFACE_STYLE_FILL_AREA ( #13487 ) ;
#5132 = DIRECTION ( 'NONE',  ( 1.000000000000000000, 0.000000000000000000, 0.000000000000000000 ) ) ;
#5133 = ADVANCED_FACE ( 'NONE', ( #623 ), #4410, .T. ) ;
#5134 = LINE ( 'NONE', #6191, #2892 ) ;
#5135 = CIRCLE ( 'NONE', #11245, 4.000000000000000000 ) ;
#5136 = EDGE_CURVE ( 'NONE', #6170, #7177, #4818, .T. ) ;
#5137 = ORIENTED_EDGE ( 'NONE', *, *, #14543, .T. ) ;
#5138 = DIRECTION ( 'NONE',  ( -0.2314933715733012709, 0.9728364810787193395, 0.000000000000000000 ) ) ;
#5139 = DIRECTION ( 'NONE',  ( 5.339417856040273846E-17, 1.063174570779084847E-17, -1.000000000000000000 ) ) ;
#5140 = CARTESIAN_POINT ( 'NONE',  ( -2.179313406705571952E-17, -18.34424029220099683, -15.96500990068145853 ) ) ;
#5141 = FACE_OUTER_BOUND ( 'NONE', #8308, .T. ) ;
#5142 = ORIENTED_EDGE ( 'NONE', *, *, #12019, .F. ) ;
#5143 = EDGE_CURVE ( 'NONE', #5459, #1104, #6692, .T. ) ;
#5144 = ORIENTED_EDGE ( 'NONE', *, *, #3148, .F. ) ;
#5145 = VERTEX_POINT ( 'NONE', #10802 ) ;
#5146 = AXIS2_PLACEMENT_3D ( 'NONE', #494, #9729, #14430 ) ;
#5147 = CIRCLE ( 'NONE', #6607, 2.999999999999988898 ) ;
#5148 = FACE_OUTER_BOUND ( 'NONE', #10538, .T. ) ;
#5149 = CIRCLE ( 'NONE', #10777, 5.400000000000000355 ) ;
#5150 = DIRECTION ( 'NONE',  ( 0.000000000000000000, 0.000000000000000000, 1.000000000000000000 ) ) ;
#5151 = CARTESIAN_POINT ( 'NONE',  ( 2.765633920072242624, -22.71065055754459650, 9.836394144775621129 ) ) ;
#5152 = CARTESIAN_POINT ( 'NONE',  ( -7.666496192563591389E-15, 11.12243880662613371, 8.842327429719135878 ) ) ;
#5153 = DIRECTION ( 'NONE',  ( -1.000000000000000000, 0.000000000000000000, 0.000000000000000000 ) ) ;
#5154 = FACE_OUTER_BOUND ( 'NONE', #2589, .T. ) ;
#5155 = EDGE_CURVE ( 'NONE', #9636, #1316, #6189, .T. ) ;
#5156 = ORIENTED_EDGE ( 'NONE', *, *, #5165, .T. ) ;
#5157 = DIRECTION ( 'NONE',  ( 0.000000000000000000, 0.000000000000000000, 1.000000000000000000 ) ) ;
#5158 = CARTESIAN_POINT ( 'NONE',  ( 2.764680872515351773, 11.36963888406687317, 9.232963481057801403 ) ) ;
#5159 = ORIENTED_EDGE ( 'NONE', *, *, #5870, .F. ) ;
#5160 = DIRECTION ( 'NONE',  ( 1.000000000000000000, 0.000000000000000000, 0.000000000000000000 ) ) ;
#5161 = CARTESIAN_POINT ( 'NONE',  ( -4.747884751462026820, -5.143694235355983579, 0.000000000000000000 ) ) ;
#5162 = CIRCLE ( 'NONE', #9324, 24.12539914357697768 ) ;
#5163 = CARTESIAN_POINT ( 'NONE',  ( 55.83172393217232354, 8.817765129169439220, 2.999999999999999112 ) ) ;
#5164 = ORIENTED_EDGE ( 'NONE', *, *, #5328, .F. ) ;
#5165 = EDGE_CURVE ( 'NONE', #5688, #3069, #12732, .T. ) ;
#5166 = DIRECTION ( 'NONE',  ( 0.000000000000000000, 0.000000000000000000, 1.000000000000000000 ) ) ;
#5167 = FACE_OUTER_BOUND ( 'NONE', #2936, .T. ) ;
#5168 = ORIENTED_EDGE ( 'NONE', *, *, #12465, .F. ) ;
#5169 = ORIENTED_EDGE ( 'NONE', *, *, #5705, .F. ) ;
#5170 = ORIENTED_EDGE ( 'NONE', *, *, #9384, .T. ) ;
#5171 = CARTESIAN_POINT ( 'NONE',  ( 3.160591952521659032, -3.281206521718069258, -0.8000000000000000444 ) ) ;
#5172 = EDGE_CURVE ( 'NONE', #4384, #7177, #3016, .T. ) ;
#5173 = CARTESIAN_POINT ( 'NONE',  ( 0.000000000000000000, 0.000000000000000000, 4.000000000000000000 ) ) ;
#5174 = CARTESIAN_POINT ( 'NONE',  ( -18.40394475573011945, -10.79473832354794460, -2.999999999999999556 ) ) ;
#5175 = CARTESIAN_POINT ( 'NONE',  ( -14.40394475573012301, -7.794738323547949932, 20.00000000000000000 ) ) ;
#5176 = LINE ( 'NONE', #9844, #11396 ) ;
#5177 = EDGE_CURVE ( 'NONE', #6579, #4492, #255, .T. ) ;
#5178 = EDGE_CURVE ( 'NONE', #9228, #2441, #10871, .T. ) ;
#5179 = CARTESIAN_POINT ( 'NONE',  ( 2.789999999999999147, 2.680914349914567470E-13, -25.59481291497571220 ) ) ;
#5180 = ORIENTED_EDGE ( 'NONE', *, *, #10953, .T. ) ;
#5181 = FACE_OUTER_BOUND ( 'NONE', #11108, .T. ) ;
#5182 = CIRCLE ( 'NONE', #7087, 6.000000000000000000 ) ;
#5183 = ORIENTED_EDGE ( 'NONE', *, *, #7853, .F. ) ;
#5184 = ORIENTED_EDGE ( 'NONE', *, *, #9459, .T. ) ;
#5185 = ADVANCED_FACE ( 'NONE', ( #13175 ), #8088, .T. ) ;
#5186 = FACE_OUTER_BOUND ( 'NONE', #8298, .T. ) ;
#5187 = ADVANCED_FACE ( 'NONE', ( #12307 ), #543, .F. ) ;
#5188 = EDGE_LOOP ( 'NONE', ( #8642, #10229, #2864, #12517 ) ) ;
#5189 = ADVANCED_FACE ( 'NONE', ( #14628 ), #14714, .T. ) ;
#5190 = UNCERTAINTY_MEASURE_WITH_UNIT (LENGTH_MEASURE( 1.000000000000000082E-05 ), #5513, 'distance_accuracy_value', 'NONE');
#5191 = DIRECTION ( 'NONE',  ( 1.000000000000000000, 0.000000000000000000, 0.000000000000000000 ) ) ;
#5192 = ORIENTED_EDGE ( 'NONE', *, *, #14364, .T. ) ;
#5193 = CARTESIAN_POINT ( 'NONE',  ( -0.4472135954999577612, 0.000000000000000000, 0.000000000000000000 ) ) ;
#5194 = CARTESIAN_POINT ( 'NONE',  ( 2.764680872515352661, -14.46287784598615644, -2.311161484776706576 ) ) ;
#5195 = EDGE_CURVE ( 'NONE', #2455, #13761, #11271, .T. ) ;
#5196 = CARTESIAN_POINT ( 'NONE',  ( 1.394999999999999574, -19.67366047555515607, -20.02152543075367319 ) ) ;
#5197 = CARTESIAN_POINT ( 'NONE',  ( 0.1855656748306449277, 2.851997810082009366, -25.77772010606602748 ) ) ;
#5198 = DIRECTION ( 'NONE',  ( 0.000000000000000000, 0.000000000000000000, 1.000000000000000000 ) ) ;
#5199 = ORIENTED_EDGE ( 'NONE', *, *, #14220, .T. ) ;
#5200 = DIRECTION ( 'NONE',  ( 0.000000000000000000, 0.000000000000000000, 1.000000000000000000 ) ) ;
#5201 = DIRECTION ( 'NONE',  ( -0.000000000000000000, -0.000000000000000000, 1.000000000000000000 ) ) ;
#5202 = VERTEX_POINT ( 'NONE', #12764 ) ;
#5203 = ORIENTED_EDGE ( 'NONE', *, *, #8888, .T. ) ;
#5204 = FACE_BOUND ( 'NONE', #12231, .T. ) ;
#5205 = FACE_OUTER_BOUND ( 'NONE', #5289, .T. ) ;
#5206 =( LENGTH_UNIT ( ) NAMED_UNIT ( * ) SI_UNIT ( .MILLI., .METRE. ) );
#5207 = DIRECTION ( 'NONE',  ( 0.000000000000000000, 0.000000000000000000, 1.000000000000000000 ) ) ;
#5208 = DIRECTION ( 'NONE',  ( 0.000000000000000000, 0.000000000000000000, 1.000000000000000000 ) ) ;
#5209 = EDGE_LOOP ( 'NONE', ( #1708, #700, #14680, #8165 ) ) ;
#5210 = DIRECTION ( 'NONE',  ( 0.000000000000000000, 0.000000000000000000, -1.000000000000000000 ) ) ;
#5211 = B_SPLINE_CURVE_WITH_KNOTS ( 'NONE', 3,
 ( #6157, #12225, #9911, #608 ),
 .UNSPECIFIED., .F., .F.,
 ( 4, 4 ),
 ( 2.135345996334758909E-07, 0.0006888010880211141137 ),
 .UNSPECIFIED. ) ;
#5212 = LINE ( 'NONE', #6347, #14289 ) ;
#5213 = CARTESIAN_POINT ( 'NONE',  ( 2.789999999999999147, 9.999777909379933050, 11.07980565117283689 ) ) ;
#5214 = ORIENTED_EDGE ( 'NONE', *, *, #4103, .T. ) ;
#5215 = ORIENTED_EDGE ( 'NONE', *, *, #6838, .F. ) ;
#5216 = VERTEX_POINT ( 'NONE', #5709 ) ;
#5217 = CYLINDRICAL_SURFACE ( 'NONE', #12206, 1.999999999999998668 ) ;
#5218 = DIRECTION ( 'NONE',  ( 1.000000000000000000, 0.000000000000000000, 0.000000000000000000 ) ) ;
#5219 = EDGE_CURVE ( 'NONE', #5377, #8463, #4411, .T. ) ;
#5220 = CARTESIAN_POINT ( 'NONE',  ( 0.000000000000000000, 0.000000000000000000, 10.00000000000000000 ) ) ;
#5221 = DIRECTION ( 'NONE',  ( -1.000000000000000000, 0.000000000000000000, -0.000000000000000000 ) ) ;
#5222 = APPLICATION_PROTOCOL_DEFINITION ( 'draft international standard', 'automotive_design', 1998, #13910 ) ;
#5223 = CARTESIAN_POINT ( 'NONE',  ( 2.789999999999999147, -14.59528211760000005, -3.120158876139185189 ) ) ;
#5224 = DIRECTION ( 'NONE',  ( -0.000000000000000000, -0.000000000000000000, -1.000000000000000000 ) ) ;
#5225 = CARTESIAN_POINT ( 'NONE',  ( 2.789999999999999147, -13.40591150984221080, -7.739906618939849103 ) ) ;
#5226 = ORIENTED_EDGE ( 'NONE', *, *, #8918, .T. ) ;
#5227 = DIRECTION ( 'NONE',  ( -1.000000000000000000, 0.000000000000000000, 0.000000000000000000 ) ) ;
#5228 = AXIS2_PLACEMENT_3D ( 'NONE', #1506, #12097, #3894 ) ;
#5229 = CARTESIAN_POINT ( 'NONE',  ( 1.894165461959355756, 24.59696699259432151, 12.96989951879416303 ) ) ;
#5230 = CARTESIAN_POINT ( 'NONE',  ( -6.124749847962873057E-14, -5.211197193340786349, 13.21862218141514411 ) ) ;
#5231 = ORIENTED_EDGE ( 'NONE', *, *, #4915, .F. ) ;
#5232 = CARTESIAN_POINT ( 'NONE',  ( 2.764680872515352661, -9.232963481057844035, 11.36963888406684298 ) ) ;
#5233 = DIRECTION ( 'NONE',  ( -1.000000000000000000, -0.000000000000000000, -0.000000000000000000 ) ) ;
#5234 = VERTEX_POINT ( 'NONE', #7932 ) ;
#5235 = VERTEX_POINT ( 'NONE', #2173 ) ;
#5236 = LINE ( 'NONE', #14603, #6312 ) ;
#5237 = DIRECTION ( 'NONE',  ( 1.000000000000000000, 0.000000000000000000, 0.000000000000000000 ) ) ;
#5238 = AXIS2_PLACEMENT_3D ( 'NONE', #10387, #2249, #12693 ) ;
#5239 = FACE_OUTER_BOUND ( 'NONE', #7350, .T. ) ;
#5240 = DIRECTION ( 'NONE',  ( -1.000000000000000000, -0.000000000000000000, -0.000000000000000000 ) ) ;
#5241 = DIRECTION ( 'NONE',  ( -1.000000000000000000, -0.000000000000000000, -0.000000000000000000 ) ) ;
#5242 = EDGE_CURVE ( 'NONE', #11722, #10930, #8090, .T. ) ;
#5243 = CARTESIAN_POINT ( 'NONE',  ( 91.12964445316929130, 15.08873975234342701, 6.000000000000000000 ) ) ;
#5244 = ORIENTED_EDGE ( 'NONE', *, *, #2417, .T. ) ;
#5245 = CARTESIAN_POINT ( 'NONE',  ( 0.000000000000000000, -7.909232158574647009, -24.34211360614308006 ) ) ;
#5246 = CARTESIAN_POINT ( 'NONE',  ( 72.68384697807672978, 11.35494834827056110, -2.000000000000000888 ) ) ;
#5247 = EDGE_CURVE ( 'NONE', #6110, #7127, #3576, .T. ) ;
#5248 = ADVANCED_FACE ( 'NONE', ( #6701 ), #14856, .T. ) ;
#5249 = EDGE_CURVE ( 'NONE', #12118, #2773, #2850, .T. ) ;
#5250 = ORIENTED_EDGE ( 'NONE', *, *, #9934, .T. ) ;
#5251 = ORIENTED_EDGE ( 'NONE', *, *, #12595, .F. ) ;
#5252 = ORIENTED_EDGE ( 'NONE', *, *, #163, .F. ) ;
#5253 = DIRECTION ( 'NONE',  ( -1.000000000000000000, 0.000000000000000000, -0.000000000000000000 ) ) ;
#5254 = DIRECTION ( 'NONE',  ( 0.000000000000000000, 0.000000000000000000, -1.000000000000000000 ) ) ;
#5255 = EDGE_LOOP ( 'NONE', ( #12377, #5345, #6749, #2187 ) ) ;
#5256 = DIRECTION ( 'NONE',  ( -1.000000000000000000, 0.000000000000000000, 0.000000000000000000 ) ) ;
#5257 = DIRECTION ( 'NONE',  ( 0.000000000000000000, 0.000000000000000000, 1.000000000000000000 ) ) ;
#5258 = B_SPLINE_CURVE_WITH_KNOTS ( 'NONE', 3,
 ( #11570, #11791, #4597, #14107 ),
 .UNSPECIFIED., .F., .F.,
 ( 4, 4 ),
 ( 2.324263106244687463E-07, 0.0006888201370294697295 ),
 .UNSPECIFIED. ) ;
#5259 = ORIENTED_EDGE ( 'NONE', *, *, #14729, .F. ) ;
#5260 = DIRECTION ( 'NONE',  ( -1.576560579138138762E-17, 1.359337748750801608E-17, -1.000000000000000000 ) ) ;
#5261 = DIRECTION ( 'NONE',  ( 0.000000000000000000, 0.000000000000000000, -1.000000000000000000 ) ) ;
#5262 = EDGE_CURVE ( 'NONE', #5463, #40, #5647, .T. ) ;
#5263 = EDGE_CURVE ( 'NONE', #13607, #11809, #859, .T. ) ;
#5264 =( GEOMETRIC_REPRESENTATION_CONTEXT ( 3 ) GLOBAL_UNCERTAINTY_ASSIGNED_CONTEXT ( ( #12234 ) ) GLOBAL_UNIT_ASSIGNED_CONTEXT ( ( #1517, #13653, #7664 ) ) REPRESENTATION_CONTEXT ( 'NONE', 'WORKASPACE' ) );
#5265 = DIRECTION ( 'NONE',  ( -0.000000000000000000, -0.000000000000000000, -1.000000000000000000 ) ) ;
#5266 = CARTESIAN_POINT ( 'NONE',  ( 72.49759028996471955, 17.18292470770558822, 2.999999999999999112 ) ) ;
#5267 = EDGE_CURVE ( 'NONE', #6623, #11577, #4689, .T. ) ;
#5268 = DIRECTION ( 'NONE',  ( -0.000000000000000000, 0.000000000000000000, 1.000000000000000000 ) ) ;
#5269 = VECTOR ( 'NONE', #10452, 1000.000000000000000 ) ;
#5270 = EDGE_LOOP ( 'NONE', ( #12158, #9617, #11837, #8392 ) ) ;
#5271 = CARTESIAN_POINT ( 'NONE',  ( 4.000000000000000888, 4.898587196589413815E-16, 6.999999999999989342 ) ) ;
#5272 = CARTESIAN_POINT ( 'NONE',  ( -4.000000000000000000, 0.000000000000000000, 6.000000000000000000 ) ) ;
#5273 = AXIS2_PLACEMENT_3D ( 'NONE', #12039, #1521, #1601 ) ;
#5274 = ORIENTED_EDGE ( 'NONE', *, *, #3525, .T. ) ;
#5275 = ORIENTED_EDGE ( 'NONE', *, *, #13403, .T. ) ;
#5276 = CARTESIAN_POINT ( 'NONE',  ( -5.435144416706554624E-16, -9.514945144208892813, 22.37986894186668962 ) ) ;
#5277 = CARTESIAN_POINT ( 'NONE',  ( 76.00000000000000000, 4.898587196589420717E-16, -131.1575142076926852 ) ) ;
#5278 = EDGE_CURVE ( 'NONE', #1971, #1373, #780, .T. ) ;
#5279 =( NAMED_UNIT ( * ) PLANE_ANGLE_UNIT ( ) SI_UNIT ( $, .RADIAN. ) );
#5280 = CARTESIAN_POINT ( 'NONE',  ( 0.5321745407694753460, 26.58873630738052185, 4.993157874727903511 ) ) ;
#5281 = AXIS2_PLACEMENT_3D ( 'NONE', #7985, #13902, #8066 ) ;
#5282 = CARTESIAN_POINT ( 'NONE',  ( 2.718131885465892683, -18.89333555428565603, 16.91241718341992240 ) ) ;
#5283 = VECTOR ( 'NONE', #8994, 1000.000000000000000 ) ;
#5284 = VERTEX_POINT ( 'NONE', #3098 ) ;
#5285 = CARTESIAN_POINT ( 'NONE',  ( 0.000000000000000000, 0.000000000000000000, 0.000000000000000000 ) ) ;
#5286 = B_SPLINE_CURVE_WITH_KNOTS ( 'NONE', 3,
 ( #12398, #1796, #14564, #4109, #553, #3957, #7713, #8632 ),
 .UNSPECIFIED., .F., .F.,
 ( 4, 2, 2, 4 ),
 ( 1.984117563342395502E-07, 0.001895214258086350351, 0.002842722181251363528, 0.003790230104416376488 ),
 .UNSPECIFIED. ) ;
#5287 = CARTESIAN_POINT ( 'NONE',  ( 2.321707774797442170, -4.824281976789052351, -0.8000000000000000444 ) ) ;
#5288 = ORIENTED_EDGE ( 'NONE', *, *, #15201, .F. ) ;
#5289 = EDGE_LOOP ( 'NONE', ( #508, #9000, #8416, #13275 ) ) ;
#5290 = ORIENTED_EDGE ( 'NONE', *, *, #14032, .T. ) ;
#5291 = VECTOR ( 'NONE', #1014, 1000.000000000000000 ) ;
#5292 = AXIS2_PLACEMENT_3D ( 'NONE', #10991, #2844, #12130 ) ;
#5293 = EDGE_LOOP ( 'NONE', ( #14237, #10622, #6350, #5684 ) ) ;
#5294 = FACE_OUTER_BOUND ( 'NONE', #4067, .T. ) ;
#5295 = CARTESIAN_POINT ( 'NONE',  ( 1.039999999999997593, 0.000000000000000000, 0.000000000000000000 ) ) ;
#5296 = CYLINDRICAL_SURFACE ( 'NONE', #14910, 4.000000000000000888 ) ;
#5297 = FACE_OUTER_BOUND ( 'NONE', #12028, .T. ) ;
#5298 = CONTEXT_DEPENDENT_SHAPE_REPRESENTATION ( #2714, #12771 ) ;
#5299 = DIRECTION ( 'NONE',  ( -1.000000000000000000, -0.000000000000000000, -0.000000000000000000 ) ) ;
#5300 = PRODUCT_DEFINITION_SHAPE ( 'NONE', 'NONE',  #6837 ) ;
#5301 = FACE_OUTER_BOUND ( 'NONE', #7013, .T. ) ;
#5302 = CARTESIAN_POINT ( 'NONE',  ( -17.83201772771817772, -12.43434672152745613, -2.999999999999999556 ) ) ;
#5303 = AXIS2_PLACEMENT_3D ( 'NONE', #10258, #14958, #2186 ) ;
#5304 = ORIENTED_EDGE ( 'NONE', *, *, #8552, .F. ) ;
#5305 = CARTESIAN_POINT ( 'NONE',  ( 0.000000000000000000, 0.000000000000000000, 6.000000000000000000 ) ) ;
#5306 = CYLINDRICAL_SURFACE ( 'NONE', #14786, 13.19999999999999929 ) ;
#5307 = AXIS2_PLACEMENT_3D ( 'NONE', #4795, #11912, #7164 ) ;
#5308 = CARTESIAN_POINT ( 'NONE',  ( 0.02531912748464587928, -5.229914364928447412, 13.68080036884346917 ) ) ;
#5309 = VERTEX_POINT ( 'NONE', #10085 ) ;
#5310 = EDGE_CURVE ( 'NONE', #3792, #3345, #7365, .T. ) ;
#5311 = LINE ( 'NONE', #12518, #5326 ) ;
#5312 = DIRECTION ( 'NONE',  ( -1.000000000000000000, 0.000000000000000000, -0.000000000000000000 ) ) ;
#5313 = VERTEX_POINT ( 'NONE', #15012 ) ;
#5314 = VERTEX_POINT ( 'NONE', #8925 ) ;
#5315 = PRESENTATION_STYLE_ASSIGNMENT (( #11212 ) ) ;
#5316 = AXIS2_PLACEMENT_3D ( 'NONE', #12069, #11998, #8688 ) ;
#5317 = CYLINDRICAL_SURFACE ( 'NONE', #9267, 8.400000000000000355 ) ;
#5318 = AXIS2_PLACEMENT_3D ( 'NONE', #2252, #868, #14865 ) ;
#5319 = CYLINDRICAL_SURFACE ( 'NONE', #7078, 13.19999999999999929 ) ;
#5320 = DIRECTION ( 'NONE',  ( -1.000000000000000000, -0.000000000000000000, -0.000000000000000000 ) ) ;
#5321 = PLANE ( 'NONE',  #14351 ) ;
#5322 = CARTESIAN_POINT ( 'NONE',  ( 0.000000000000000000, 0.000000000000000000, 1.395000000000000462 ) ) ;
#5323 = EDGE_CURVE ( 'NONE', #8601, #1485, #4479, .T. ) ;
#5324 = ORIENTED_EDGE ( 'NONE', *, *, #2107, .T. ) ;
#5325 = CARTESIAN_POINT ( 'NONE',  ( 14.40394475573011945, -10.79473832354794460, 5.500000000000000000 ) ) ;
#5326 = VECTOR ( 'NONE', #4295, 1000.000000000000000 ) ;
#5327 = CARTESIAN_POINT ( 'NONE',  ( -14.40394475573011945, -10.79473832354794460, 12.00000000000000000 ) ) ;
#5328 = EDGE_CURVE ( 'NONE', #14141, #11359, #3932, .T. ) ;
#5329 = ORIENTED_EDGE ( 'NONE', *, *, #3917, .T. ) ;
#5330 = PRESENTATION_LAYER_ASSIGNMENT (  '', '', ( #1143 ) ) ;
#5331 = EDGE_CURVE ( 'NONE', #13989, #4548, #3401, .T. ) ;
#5332 = EDGE_LOOP ( 'NONE', ( #7589, #14128 ) ) ;
#5333 = VERTEX_POINT ( 'NONE', #13616 ) ;
#5334 = VERTEX_POINT ( 'NONE', #6632 ) ;
#5335 = CARTESIAN_POINT ( 'NONE',  ( 1.998465710409312357E-16, 22.37986894186671805, 9.514945144208807548 ) ) ;
#5336 = CARTESIAN_POINT ( 'NONE',  ( -9.999999999999998224, 0.000000000000000000, 3.000000000000002665 ) ) ;
#5337 = AXIS2_PLACEMENT_3D ( 'NONE', #3385, #8074, #2230 ) ;
#5338 = VECTOR ( 'NONE', #11247, 1000.000000000000000 ) ;
#5339 = UNCERTAINTY_MEASURE_WITH_UNIT (LENGTH_MEASURE( 1.000000000000000082E-05 ), #10257, 'distance_accuracy_value', 'NONE');
#5340 = COLOUR_RGB ( '',1.000000000000000000, 0.9490196078431372140, 0.9098039215686274384 ) ;
#5341 = CARTESIAN_POINT ( 'NONE',  ( 13.78117670802322259, -24.07785181381190753, -2.000000000000000000 ) ) ;
#5342 = VECTOR ( 'NONE', #2492, 1000.000000000000000 ) ;
#5343 = DIRECTION ( 'NONE',  ( -0.000000000000000000, -0.000000000000000000, 1.000000000000000000 ) ) ;
#5344 = ADVANCED_FACE ( 'NONE', ( #5487 ), #10159, .T. ) ;
#5345 = ORIENTED_EDGE ( 'NONE', *, *, #10742, .F. ) ;
#5346 = EDGE_CURVE ( 'NONE', #7127, #13239, #14229, .T. ) ;
#5347 = CARTESIAN_POINT ( 'NONE',  ( 1.039999999999996705, 27.76164181293051669, -4.147968289691385202 ) ) ;
#5348 = DIRECTION ( 'NONE',  ( 1.000000000000000000, 0.000000000000000000, 0.000000000000000000 ) ) ;
#5349 = FACE_OUTER_BOUND ( 'NONE', #6563, .T. ) ;
#5350 =( GEOMETRIC_REPRESENTATION_CONTEXT ( 3 ) GLOBAL_UNCERTAINTY_ASSIGNED_CONTEXT ( ( #13840 ) ) GLOBAL_UNIT_ASSIGNED_CONTEXT ( ( #6421, #11104, #566 ) ) REPRESENTATION_CONTEXT ( 'NONE', 'WORKASPACE' ) );
#5351 = LINE ( 'NONE', #13707, #4955 ) ;
#5352 = DIRECTION ( 'NONE',  ( -1.000000000000000000, 0.000000000000000000, 0.000000000000000000 ) ) ;
#5353 = AXIS2_PLACEMENT_3D ( 'NONE', #8001, #12681, #777 ) ;
#5354 = VERTEX_POINT ( 'NONE', #10615 ) ;
#5355 = VECTOR ( 'NONE', #1747, 1000.000000000000000 ) ;
#5356 = CARTESIAN_POINT ( 'NONE',  ( 18.87754531448929995, -24.24225080111726527, 5.000000000000000000 ) ) ;
#5357 = DIRECTION ( 'NONE',  ( -0.000000000000000000, -0.000000000000000000, -1.000000000000000000 ) ) ;
#5358 = AXIS2_PLACEMENT_3D ( 'NONE', #10234, #5636, #14936 ) ;
#5359 = ORIENTED_EDGE ( 'NONE', *, *, #2204, .F. ) ;
#5360 = ORIENTED_EDGE ( 'NONE', *, *, #9566, .F. ) ;
#5361 = CARTESIAN_POINT ( 'NONE',  ( -2.321707774797442170, -4.824281976789052351, -0.8000000000000000444 ) ) ;
#5362 = EDGE_CURVE ( 'NONE', #12400, #9201, #2665, .T. ) ;
#5363 = CARTESIAN_POINT ( 'NONE',  ( 13.28797974610715116, -21.11867004231547540, 6.000000000000000000 ) ) ;
#5364 = EDGE_CURVE ( 'NONE', #5007, #14821, #14070, .T. ) ;
#5365 = EDGE_CURVE ( 'NONE', #1234, #14323, #7427, .T. ) ;
#5366 = CARTESIAN_POINT ( 'NONE',  ( 2.789999999999999147, 7.739906618939895289, -10.88091150984218380 ) ) ;
#5367 =( GEOMETRIC_REPRESENTATION_CONTEXT ( 3 ) GLOBAL_UNCERTAINTY_ASSIGNED_CONTEXT ( ( #11007 ) ) GLOBAL_UNIT_ASSIGNED_CONTEXT ( ( #253, #12255, #1655 ) ) REPRESENTATION_CONTEXT ( 'NONE', 'WORKASPACE' ) );
#5368 = ORIENTED_EDGE ( 'NONE', *, *, #14561, .T. ) ;
#5369 = CARTESIAN_POINT ( 'NONE',  ( 1.150000000000000577, 0.000000000000000000, 0.000000000000000000 ) ) ;
#5370 = CARTESIAN_POINT ( 'NONE',  ( 1.394999999999999574, 17.29145405592688789, 4.835383649608534284 ) ) ;
#5371 = CIRCLE ( 'NONE', #9036, 4.999999999999997335 ) ;
#5372 = VECTOR ( 'NONE', #436, 1000.000000000000000 ) ;
#5373 = ORIENTED_EDGE ( 'NONE', *, *, #14707, .T. ) ;
#5374 = DIRECTION ( 'NONE',  ( 0.000000000000000000, -0.5000000000000007772, 0.8660254037844381525 ) ) ;
#5375 = ORIENTED_EDGE ( 'NONE', *, *, #13221, .F. ) ;
#5376 = ORIENTED_EDGE ( 'NONE', *, *, #8164, .T. ) ;
#5377 = VERTEX_POINT ( 'NONE', #1167 ) ;
#5378 = CARTESIAN_POINT ( 'NONE',  ( 2.789999999999999147, 24.44424927289185945, -0.2301004812058395077 ) ) ;
#5379 = DIRECTION ( 'NONE',  ( -1.000000000000000000, 0.000000000000000000, 0.000000000000000000 ) ) ;
#5380 = CARTESIAN_POINT ( 'NONE',  ( 2.031033471609899888, -3.797536611356125746, -27.31260702007179830 ) ) ;
#5381 = DIRECTION ( 'NONE',  ( 0.000000000000000000, 0.000000000000000000, 1.000000000000000000 ) ) ;
#5382 = CARTESIAN_POINT ( 'NONE',  ( 2.765633920072235963, 24.63872515616082737, 2.336989772644355146 ) ) ;
#5383 = FACE_OUTER_BOUND ( 'NONE', #3210, .T. ) ;
#5384 = CARTESIAN_POINT ( 'NONE',  ( 2.697960317788776319, 14.31435947614549242, -5.280991956246970709 ) ) ;
#5385 = ORIENTED_EDGE ( 'NONE', *, *, #3558, .F. ) ;
#5386 = CARTESIAN_POINT ( 'NONE',  ( 0.000000000000000000, -9.324097380959319281, -22.25075486061748009 ) ) ;
#5387 = CYLINDRICAL_SURFACE ( 'NONE', #3480, 5.999999999999999112 ) ;
#5388 = LINE ( 'NONE', #2986, #14353 ) ;
#5389 = EDGE_CURVE ( 'NONE', #5041, #12602, #12515, .T. ) ;
#5390 = ORIENTED_EDGE ( 'NONE', *, *, #7607, .T. ) ;
#5391 = VECTOR ( 'NONE', #3842, 1000.000000000000000 ) ;
#5392 = AXIS2_PLACEMENT_3D ( 'NONE', #1271, #189, #13968 ) ;
#5393 = CARTESIAN_POINT ( 'NONE',  ( 56.98919079003883326, 3.953582723775848962, 2.999999999999999112 ) ) ;
#5394 = DIRECTION ( 'NONE',  ( -1.000000000000000000, -0.000000000000000000, -0.000000000000000000 ) ) ;
#5395 = ORIENTED_EDGE ( 'NONE', *, *, #434, .F. ) ;
#5396 = ORIENTED_EDGE ( 'NONE', *, *, #313, .T. ) ;
#5397 = CARTESIAN_POINT ( 'NONE',  ( 0.09203968221122159343, 5.280991956247319763, -14.31435947614536275 ) ) ;
#5398 = DIRECTION ( 'NONE',  ( 0.000000000000000000, 0.000000000000000000, 1.000000000000000000 ) ) ;
#5399 = CARTESIAN_POINT ( 'NONE',  ( 80.82762530298222714, -9.999999999999994671, 6.000000000000000000 ) ) ;
#5400 = DIRECTION ( 'NONE',  ( -1.000000000000000000, 0.000000000000000000, -0.000000000000000000 ) ) ;
#5401 = DIRECTION ( 'NONE',  ( 0.000000000000000000, 0.000000000000000000, 1.000000000000000000 ) ) ;
#5402 = DIRECTION ( 'NONE',  ( 0.000000000000000000, -0.8660254037844362651, -0.5000000000000041078 ) ) ;
#5403 = DIRECTION ( 'NONE',  ( 1.000000000000000000, 0.000000000000000000, 0.000000000000000000 ) ) ;
#5404 = AXIS2_PLACEMENT_3D ( 'NONE', #5672, #8261, #1267 ) ;
#5405 = EDGE_CURVE ( 'NONE', #9117, #13730, #5162, .T. ) ;
#5406 = ORIENTED_EDGE ( 'NONE', *, *, #11003, .T. ) ;
#5407 = DIRECTION ( 'NONE',  ( 1.000000000000000000, 0.000000000000000000, 0.000000000000000000 ) ) ;
#5408 = CARTESIAN_POINT ( 'NONE',  ( 2.765633920072235963, 21.30679549418649543, -12.59161484032888723 ) ) ;
#5409 = ORIENTED_EDGE ( 'NONE', *, *, #12161, .F. ) ;
#5410 = ORIENTED_EDGE ( 'NONE', *, *, #9336, .F. ) ;
#5411 = ORIENTED_EDGE ( 'NONE', *, *, #7638, .F. ) ;
#5412 = EDGE_LOOP ( 'NONE', ( #684, #14580, #13715, #9552 ) ) ;
#5413 = AXIS2_PLACEMENT_3D ( 'NONE', #1471, #6155, #10839 ) ;
#5414 = DIRECTION ( 'NONE',  ( 0.000000000000000000, 0.000000000000000000, -1.000000000000000000 ) ) ;
#5415 = EDGE_CURVE ( 'NONE', #807, #6110, #12902, .T. ) ;
#5416 = DIRECTION ( 'NONE',  ( 0.9863939238321436376, 0.1643989873053573192, 0.000000000000000000 ) ) ;
#5417 = EDGE_CURVE ( 'NONE', #9595, #11083, #6001, .T. ) ;
#5418 = DIRECTION ( 'NONE',  ( -1.000000000000000000, -0.000000000000000000, 0.000000000000000000 ) ) ;
#5419 = EDGE_LOOP ( 'NONE', ( #6375, #9137, #9506, #6662, #12173, #120, #9828, #13316 ) ) ;
#5420 = CARTESIAN_POINT ( 'NONE',  ( 2.765633920072235519, -9.836394144775869819, 22.71065055754449347 ) ) ;
#5421 = CARTESIAN_POINT ( 'NONE',  ( 0.006930995026450773554, -23.92277630352799278, 5.408431875071351591 ) ) ;
#5422 = VECTOR ( 'NONE', #3380, 1000.000000000000000 ) ;
#5423 = CARTESIAN_POINT ( 'NONE',  ( 1.039999999999997815, 17.29145405592688789, 4.835383649608532508 ) ) ;
#5424 = CARTESIAN_POINT ( 'NONE',  ( 93.34550147531103903, 3.654933296868752457, 2.999999999999999112 ) ) ;
#5425 = ORIENTED_EDGE ( 'NONE', *, *, #2129, .F. ) ;
#5426 = CARTESIAN_POINT ( 'NONE',  ( 0.02531912748464674665, -11.36963888406694068, 9.232963481057725019 ) ) ;
#5427 = CARTESIAN_POINT ( 'NONE',  ( 2.582362745529150683, -12.04200105039462976, -10.30022894898818464 ) ) ;
#5428 = ORIENTED_EDGE ( 'NONE', *, *, #1210, .T. ) ;
#5429 = VERTEX_POINT ( 'NONE', #14001 ) ;
#5430 = DIRECTION ( 'NONE',  ( 0.000000000000000000, 0.000000000000000000, 1.000000000000000000 ) ) ;
#5431 = FACE_OUTER_BOUND ( 'NONE', #5209, .T. ) ;
#5432 = ORIENTED_EDGE ( 'NONE', *, *, #9553, .T. ) ;
#5433 = EDGE_CURVE ( 'NONE', #9763, #2063, #2474, .T. ) ;
#5434 = CARTESIAN_POINT ( 'NONE',  ( 2.790000000000008029, -8.842327429719018639, -11.12243880662622431 ) ) ;
#5435 = VERTEX_POINT ( 'NONE', #5865 ) ;
#5436 = DIRECTION ( 'NONE',  ( 0.000000000000000000, 0.000000000000000000, -1.000000000000000000 ) ) ;
#5437 = LINE ( 'NONE', #14656, #8386 ) ;
#5438 = VERTEX_POINT ( 'NONE', #14231 ) ;
#5439 = CARTESIAN_POINT ( 'NONE',  ( 0.7589665203264078785, 19.12621924769895898, -19.86422722021291776 ) ) ;
#5440 = CARTESIAN_POINT ( 'NONE',  ( 0.2818303507154712451, 3.072260951847531008, 15.84037596932109615 ) ) ;
#5441 = ORIENTED_EDGE ( 'NONE', *, *, #14955, .T. ) ;
#5442 = ADVANCED_FACE ( 'NONE', ( #1240 ), #4942, .T. ) ;
#5443 = EDGE_CURVE ( 'NONE', #3508, #6870, #4488, .T. ) ;
#5444 = ORIENTED_EDGE ( 'NONE', *, *, #3302, .T. ) ;
#5445 = CARTESIAN_POINT ( 'NONE',  ( 2.765633920072235963, -5.391175441198450713, -24.15498966839968276 ) ) ;
#5446 = DIRECTION ( 'NONE',  ( 0.000000000000000000, 0.000000000000000000, 1.000000000000000000 ) ) ;
#5447 = CARTESIAN_POINT ( 'NONE',  ( 56.98919079003883326, 3.953582723775848962, -2.000000000000000888 ) ) ;
#5448 = CARTESIAN_POINT ( 'NONE',  ( 2.740740100656034794, 13.98927362834316135, 5.263697681271602313 ) ) ;
#5449 = CONTEXT_DEPENDENT_SHAPE_REPRESENTATION ( #149, #998 ) ;
#5450 = FACE_OUTER_BOUND ( 'NONE', #528, .T. ) ;
#5451 = PLANE ( 'NONE',  #13253 ) ;
#5452 = DIRECTION ( 'NONE',  ( -1.000000000000000000, 0.000000000000000000, 0.000000000000000000 ) ) ;
#5453 = ORIENTED_EDGE ( 'NONE', *, *, #2799, .F. ) ;
#5454 = CARTESIAN_POINT ( 'NONE',  ( 2.740003288479521792, 2.439987328297174241, -14.75565684666123900 ) ) ;
#5455 = DIRECTION ( 'NONE',  ( -1.000000000000000000, 0.000000000000000000, -0.000000000000000000 ) ) ;
#5456 = EDGE_CURVE ( 'NONE', #10374, #11429, #13464, .T. ) ;
#5457 = LINE ( 'NONE', #15051, #5095 ) ;
#5458 = EDGE_CURVE ( 'NONE', #5334, #418, #4913, .T. ) ;
#5459 = VERTEX_POINT ( 'NONE', #9845 ) ;
#5460 = ADVANCED_FACE ( 'NONE', ( #5015 ), #9907, .T. ) ;
#5461 = CARTESIAN_POINT ( 'NONE',  ( -14.40394475573012301, -13.79473832354794993, 20.00000000000000000 ) ) ;
#5462 = FACE_OUTER_BOUND ( 'NONE', #3486, .T. ) ;
#5463 = VERTEX_POINT ( 'NONE', #5097 ) ;
#5464 = VERTEX_POINT ( 'NONE', #3934 ) ;
#5465 = CARTESIAN_POINT ( 'NONE',  ( 0.000000000000000000, 0.000000000000000000, 6.999999999999989342 ) ) ;
#5466 = CARTESIAN_POINT ( 'NONE',  ( 0.000000000000000000, 0.000000000000000000, 10.00000000000000000 ) ) ;
#5467 = DIRECTION ( 'NONE',  ( 0.000000000000000000, 0.000000000000000000, 1.000000000000000000 ) ) ;
#5468 = DIRECTION ( 'NONE',  ( -1.000000000000000000, -0.000000000000000000, -0.000000000000000000 ) ) ;
#5469 = CARTESIAN_POINT ( 'NONE',  ( 4.271534284832219323E-17, 3.369532131271296443E-15, 6.999999999999989342 ) ) ;
#5470 = EDGE_CURVE ( 'NONE', #3838, #214, #12506, .T. ) ;
#5471 = CIRCLE ( 'NONE', #14038, 2.524999999999998135 ) ;
#5472 = CARTESIAN_POINT ( 'NONE',  ( 1.039999999999995373, 25.12109765559670649, -12.52377138324197681 ) ) ;
#5473 = CARTESIAN_POINT ( 'NONE',  ( 0.07186815222488118771, 24.78765742476146272, -5.344160105508446001 ) ) ;
#5474 = ORIENTED_EDGE ( 'NONE', *, *, #4943, .T. ) ;
#5475 = CARTESIAN_POINT ( 'NONE',  ( 79.18363542992867110, -10.13606076167855008, 6.000000000000000000 ) ) ;
#5476 = DIRECTION ( 'NONE',  ( 0.000000000000000000, 0.000000000000000000, 1.000000000000000000 ) ) ;
#5477 = EDGE_LOOP ( 'NONE', ( #13122, #4208, #7512, #5801 ) ) ;
#5478 = SHAPE_REPRESENTATION_RELATIONSHIP ( 'NONE' , 'NONE' ,  #4172, #476 ) ;
#5479 = VECTOR ( 'NONE', #5494, 1000.000000000000000 ) ;
#5480 = AXIS2_PLACEMENT_3D ( 'NONE', #1891, #14966, #11181 ) ;
#5481 = ORIENTED_EDGE ( 'NONE', *, *, #8836, .F. ) ;
#5482 = VERTEX_POINT ( 'NONE', #4162 ) ;
#5483 = ORIENTED_EDGE ( 'NONE', *, *, #4879, .T. ) ;
#5484 = CYLINDRICAL_SURFACE ( 'NONE', #11459, 3.799999999999999378 ) ;
#5485 = CYLINDRICAL_SURFACE ( 'NONE', #8075, 0.5999999999999998668 ) ;
#5486 = APPLICATION_CONTEXT ( 'automotive_design' ) ;
#5487 = FACE_OUTER_BOUND ( 'NONE', #6643, .T. ) ;
#5488 = EDGE_CURVE ( 'NONE', #10393, #14849, #14479, .T. ) ;
#5489 = VERTEX_POINT ( 'NONE', #7317 ) ;
#5490 = AXIS2_PLACEMENT_3D ( 'NONE', #13245, #2725, #12245 ) ;
#5491 = CARTESIAN_POINT ( 'NONE',  ( 0.000000000000000000, -23.48180575137727288, -5.535312321042949790 ) ) ;
#5492 = CARTESIAN_POINT ( 'NONE',  ( 2.765633920072239516, -24.15498966839958683, -5.391175441198872598 ) ) ;
#5493 = DIRECTION ( 'NONE',  ( 1.000000000000000000, 0.000000000000000000, -1.576560579138137530E-17 ) ) ;
#5494 = DIRECTION ( 'NONE',  ( -0.000000000000000000, -0.000000000000000000, 1.000000000000000000 ) ) ;
#5495 = ORIENTED_EDGE ( 'NONE', *, *, #2392, .T. ) ;
#5496 = DIRECTION ( 'NONE',  ( -0.000000000000000000, -0.000000000000000000, -1.000000000000000000 ) ) ;
#5497 = CARTESIAN_POINT ( 'NONE',  ( 2.764680872515351329, -11.36963888406680923, -9.232963481057881339 ) ) ;
#5498 = VERTEX_POINT ( 'NONE', #1700 ) ;
#5499 = VERTEX_POINT ( 'NONE', #14470 ) ;
#5500 = SHAPE_REPRESENTATION_RELATIONSHIP ( 'NONE' , 'NONE' ,  #5737, #14983 ) ;
#5501 = CARTESIAN_POINT ( 'NONE',  ( 0.7589665203264103210, -19.12621924769880977, 19.86422722021305631 ) ) ;
#5502 = ORIENTED_EDGE ( 'NONE', *, *, #5195, .F. ) ;
#5503 = B_SPLINE_CURVE_WITH_KNOTS ( 'NONE', 3,
 ( #3637, #9260, #6877, #2488 ),
 .UNSPECIFIED., .F., .F.,
 ( 4, 4 ),
 ( 0.005342776758202955750, 0.005948405594583417583 ),
 .UNSPECIFIED. ) ;
#5504 = DIRECTION ( 'NONE',  ( -1.000000000000000000, 0.000000000000000000, -0.000000000000000000 ) ) ;
#5505 = ORIENTED_EDGE ( 'NONE', *, *, #12994, .F. ) ;
#5506 = CARTESIAN_POINT ( 'NONE',  ( 0.7589665203264061022, 19.86422722021312026, 19.12621924769873161 ) ) ;
#5507 = CARTESIAN_POINT ( 'NONE',  ( 0.02531912748464631296, -13.68080036884344963, -5.229914364928496262 ) ) ;
#5508 = VERTEX_POINT ( 'NONE', #8535 ) ;
#5509 = CARTESIAN_POINT ( 'NONE',  ( 0.000000000000000000, -5.535312321042921369, 23.48180575137728354 ) ) ;
#5510 = ADVANCED_FACE ( 'NONE', ( #4079 ), #14611, .F. ) ;
#5511 = ORIENTED_EDGE ( 'NONE', *, *, #11130, .F. ) ;
#5512 = ORIENTED_EDGE ( 'NONE', *, *, #11813, .F. ) ;
#5513 =( LENGTH_UNIT ( ) NAMED_UNIT ( * ) SI_UNIT ( .MILLI., .METRE. ) );
#5514 = EDGE_CURVE ( 'NONE', #8417, #910, #6494, .T. ) ;
#5515 = ORIENTED_EDGE ( 'NONE', *, *, #5470, .T. ) ;
#5516 = CARTESIAN_POINT ( 'NONE',  ( 2.764680872515354881, -13.68080036884352246, 5.229914364928304416 ) ) ;
#5517 = AXIS2_PLACEMENT_3D ( 'NONE', #13136, #1470, #8753 ) ;
#5518 = CARTESIAN_POINT ( 'NONE',  ( -9.999999999999998224, -1.390791565672605534, 3.000000000000002665 ) ) ;
#5519 = CIRCLE ( 'NONE', #6479, 3.000000000000000888 ) ;
#5520 = DIRECTION ( 'NONE',  ( -1.000000000000000000, 0.000000000000000000, -0.000000000000000000 ) ) ;
#5521 = ITEM_DEFINED_TRANSFORMATION ( 'NONE', 'NONE', #3550,  #1376 ) ;
#5522 = DIRECTION ( 'NONE',  ( 1.000000000000000000, 0.000000000000000000, 0.000000000000000000 ) ) ;
#5523 = CARTESIAN_POINT ( 'NONE',  ( 0.02436607992776021470, 21.30679549418649543, -12.59161484032888723 ) ) ;
#5524 = EDGE_CURVE ( 'NONE', #4654, #12548, #13450, .T. ) ;
#5525 = VERTEX_POINT ( 'NONE', #7546 ) ;
#5526 = EDGE_CURVE ( 'NONE', #9636, #1932, #242, .T. ) ;
#5527 = DIRECTION ( 'NONE',  ( 1.000000000000000000, 0.000000000000000000, 0.000000000000000000 ) ) ;
#5528 = VECTOR ( 'NONE', #13981, 1000.000000000000000 ) ;
#5529 = CARTESIAN_POINT ( 'NONE',  ( 18.21994936526786901, -20.29667510578869027, 4.000000000000001776 ) ) ;
#5530 = AXIS2_PLACEMENT_3D ( 'NONE', #15086, #15171, #7866 ) ;
#5531 = ORIENTED_EDGE ( 'NONE', *, *, #6724, .T. ) ;
#5532 = CIRCLE ( 'NONE', #5769, 24.12539914357697413 ) ;
#5533 = DIRECTION ( 'NONE',  ( 0.000000000000000000, 0.000000000000000000, -1.000000000000000000 ) ) ;
#5534 = CARTESIAN_POINT ( 'NONE',  ( -9.999999999999998224, 0.000000000000000000, 3.000000000000002665 ) ) ;
#5535 = VERTEX_POINT ( 'NONE', #5243 ) ;
#5536 = ORIENTED_EDGE ( 'NONE', *, *, #12554, .T. ) ;
#5537 = FACE_OUTER_BOUND ( 'NONE', #3524, .T. ) ;
#5538 = LINE ( 'NONE', #986, #8522 ) ;
#5539 = ORIENTED_EDGE ( 'NONE', *, *, #622, .T. ) ;
#5540 = DIRECTION ( 'NONE',  ( 0.000000000000000000, 0.000000000000000000, 1.000000000000000000 ) ) ;
#5541 = DIRECTION ( 'NONE',  ( 0.000000000000000000, 0.000000000000000000, 1.000000000000000000 ) ) ;
#5542 = CARTESIAN_POINT ( 'NONE',  ( 1.749999999999998002, 20.02152543075346003, 19.67366047555537634 ) ) ;
#5543 = AXIS2_PLACEMENT_3D ( 'NONE', #748, #14815, #14976 ) ;
#5544 = EDGE_CURVE ( 'NONE', #2656, #8622, #8756, .T. ) ;
#5545 = CIRCLE ( 'NONE', #865, 0.7500000000000002220 ) ;
#5546 = CARTESIAN_POINT ( 'NONE',  ( 3.160591952521659032, -3.281206521718069258, 0.000000000000000000 ) ) ;
#5547 = CARTESIAN_POINT ( 'NONE',  ( 0.1855657389739081564, 25.39738473785008210, -5.253342437939463316 ) ) ;
#5548 = EDGE_CURVE ( 'NONE', #406, #3713, #13489, .T. ) ;
#5549 = ORIENTED_EDGE ( 'NONE', *, *, #589, .F. ) ;
#5550 = DIRECTION ( 'NONE',  ( 0.000000000000000000, 0.000000000000000000, -1.000000000000000000 ) ) ;
#5551 = VERTEX_POINT ( 'NONE', #6227 ) ;
#5552 = AXIS2_PLACEMENT_3D ( 'NONE', #12, #7168, #3478 ) ;
#5553 = EDGE_CURVE ( 'NONE', #8635, #3198, #220, .T. ) ;
#5554 = SURFACE_STYLE_USAGE ( .BOTH. , #701 ) ;
#5555 = AXIS2_PLACEMENT_3D ( 'NONE', #4089, #8769, #6545 ) ;
#5556 = ORIENTED_EDGE ( 'NONE', *, *, #5526, .T. ) ;
#5557 = EDGE_LOOP ( 'NONE', ( #3749, #6480, #13478, #15007, #617, #435, #10761, #6393 ) ) ;
#5558 = EDGE_LOOP ( 'NONE', ( #9446, #11851, #490, #7750 ) ) ;
#5559 = CARTESIAN_POINT ( 'NONE',  ( 2.257825467309738432, 26.83036154824994313, 3.467596033028380376 ) ) ;
#5560 = DIRECTION ( 'NONE',  ( 0.000000000000000000, 0.000000000000000000, -1.000000000000000000 ) ) ;
#5561 = CARTESIAN_POINT ( 'NONE',  ( 1.039999999999996927, 4.633866840649313090, -27.68468304288253634 ) ) ;
#5562 = DIRECTION ( 'NONE',  ( 0.000000000000000000, 0.000000000000000000, -1.000000000000000000 ) ) ;
#5563 = AXIS2_PLACEMENT_3D ( 'NONE', #13892, #5394, #6825 ) ;
#5564 = ORIENTED_EDGE ( 'NONE', *, *, #15030, .T. ) ;
#5565 = DIRECTION ( 'NONE',  ( 0.000000000000000000, 0.000000000000000000, -1.000000000000000000 ) ) ;
#5566 = CARTESIAN_POINT ( 'NONE',  ( 83.50748565343083385, 13.38500995229612478, 2.999999999999999112 ) ) ;
#5567 = DIRECTION ( 'NONE',  ( -0.000000000000000000, -0.000000000000000000, -1.000000000000000000 ) ) ;
#5568 = EDGE_CURVE ( 'NONE', #8616, #7008, #11762, .T. ) ;
#5569 = AXIS2_PLACEMENT_3D ( 'NONE', #13277, #7528, #10824 ) ;
#5570 = EDGE_LOOP ( 'NONE', ( #3462, #2938, #1531, #5109, #1897, #712, #9801, #2271 ) ) ;
#5571 = DIRECTION ( 'NONE',  ( 1.000000000000000000, 0.000000000000000000, 0.000000000000000000 ) ) ;
#5572 = VECTOR ( 'NONE', #7977, 1000.000000000000000 ) ;
#5573 = CARTESIAN_POINT ( 'NONE',  ( 0.1882239080259267838, -25.40949241676349146, -5.251266773802644394 ) ) ;
#5574 = EDGE_LOOP ( 'NONE', ( #7452, #11220, #2692, #13629 ) ) ;
#5575 = EDGE_LOOP ( 'NONE', ( #3433, #6074 ) ) ;
#5576 = AXIS2_PLACEMENT_3D ( 'NONE', #3268, #5590, #9116 ) ;
#5577 =( NAMED_UNIT ( * ) SI_UNIT ( $, .STERADIAN. ) SOLID_ANGLE_UNIT ( ) );
#5578 = DIRECTION ( 'NONE',  ( -0.9863939238321437486, -0.1643989873053574857, 0.000000000000000000 ) ) ;
#5579 = ORIENTED_EDGE ( 'NONE', *, *, #2673, .T. ) ;
#5580 = AXIS2_PLACEMENT_3D ( 'NONE', #1912, #10350, #6604 ) ;
#5581 = AXIS2_PLACEMENT_3D ( 'NONE', #9611, #2476, #8375 ) ;
#5582 = CARTESIAN_POINT ( 'NONE',  ( 2.782650468023970092, -2.217353748341832187, -14.24968354755770861 ) ) ;
#5583 = EDGE_CURVE ( 'NONE', #10097, #7890, #296, .T. ) ;
#5584 = ORIENTED_EDGE ( 'NONE', *, *, #9700, .T. ) ;
#5585 = LINE ( 'NONE', #3203, #2270 ) ;
#5586 = AXIS2_PLACEMENT_3D ( 'NONE', #4550, #9231, #13920 ) ;
#5587 = ORIENTED_EDGE ( 'NONE', *, *, #9619, .T. ) ;
#5588 = VECTOR ( 'NONE', #9588, 1000.000000000000000 ) ;
#5589 = CARTESIAN_POINT ( 'NONE',  ( 0.1855655959470668692, 17.45907811351482763, -19.17825124759758282 ) ) ;
#5590 = DIRECTION ( 'NONE',  ( -0.8406209333187997235, -0.5416238976136762417, 0.000000000000000000 ) ) ;
#5591 = ORIENTED_EDGE ( 'NONE', *, *, #14084, .T. ) ;
#5592 = ORIENTED_EDGE ( 'NONE', *, *, #2417, .F. ) ;
#5593 = CARTESIAN_POINT ( 'NONE',  ( -14.40394475573011768, -7.794738323547949932, 16.99999999999999645 ) ) ;
#5594 = DIRECTION ( 'NONE',  ( 0.000000000000000000, 0.000000000000000000, -1.000000000000000000 ) ) ;
#5595 = EDGE_CURVE ( 'NONE', #9825, #4705, #467, .T. ) ;
#5596 = AXIS2_PLACEMENT_3D ( 'NONE', #10358, #3374, #7981 ) ;
#5597 = CARTESIAN_POINT ( 'NONE',  ( 55.83172393217232354, 8.817765129169439220, 6.000000000000000000 ) ) ;
#5598 = DIRECTION ( 'NONE',  ( 1.576560579138138762E-17, -1.359337748750801608E-17, 1.000000000000000000 ) ) ;
#5599 = CONTEXT_DEPENDENT_SHAPE_REPRESENTATION ( #6457, #2605 ) ;
#5600 = DIRECTION ( 'NONE',  ( -1.000000000000000000, 0.000000000000000000, 0.000000000000000000 ) ) ;
#5601 = EDGE_CURVE ( 'NONE', #2078, #6712, #2443, .T. ) ;
#5602 = CIRCLE ( 'NONE', #14179, 28.06981291497571007 ) ;
#5603 = DIRECTION ( 'NONE',  ( 0.7573544145849104847, -0.6530040510661075936, -2.081668171172168513E-17 ) ) ;
#5604 = VERTEX_POINT ( 'NONE', #6533 ) ;
#5605 = CYLINDRICAL_SURFACE ( 'NONE', #12958, 3.799999999999999378 ) ;
#5606 = CARTESIAN_POINT ( 'NONE',  ( 8.403944755730119454, -10.79473832354794460, 5.500000000000001776 ) ) ;
#5607 = DIRECTION ( 'NONE',  ( 1.000000000000000000, 0.000000000000000000, 0.000000000000000000 ) ) ;
#5608 = ORIENTED_EDGE ( 'NONE', *, *, #8638, .F. ) ;
#5609 = CARTESIAN_POINT ( 'NONE',  ( 88.84370878116858705, 10.64188714589527684, 7.000000000000000000 ) ) ;
#5610 = DIRECTION ( 'NONE',  ( -1.000000000000000000, -0.000000000000000000, 0.000000000000000000 ) ) ;
#5611 = VERTEX_POINT ( 'NONE', #10144 ) ;
#5612 = AXIS2_PLACEMENT_3D ( 'NONE', #2603, #207, #14945 ) ;
#5613 = EDGE_LOOP ( 'NONE', ( #13417, #7390, #11918, #7017, #13337, #1941, #2852 ) ) ;
#5614 = DIRECTION ( 'NONE',  ( -1.000000000000000000, 0.000000000000000000, -0.000000000000000000 ) ) ;
#5615 = DIRECTION ( 'NONE',  ( 0.000000000000000000, 0.000000000000000000, 1.000000000000000000 ) ) ;
#5616 = EDGE_CURVE ( 'NONE', #8705, #3394, #1962, .T. ) ;
#5617 = ORIENTED_EDGE ( 'NONE', *, *, #5524, .F. ) ;
#5618 = CARTESIAN_POINT ( 'NONE',  ( 1.749999999999999778, -17.39253030560844948, 4.458161950358431547 ) ) ;
#5619 = CARTESIAN_POINT ( 'NONE',  ( 64.00448238961524794, 36.25062540154047497, -2.000000000000000000 ) ) ;
#5620 = DIRECTION ( 'NONE',  ( -0.4571871344001416926, -0.8893705212896291235, 0.000000000000000000 ) ) ;
#5621 = CARTESIAN_POINT ( 'NONE',  ( 0.5279273620711166792, -12.96450951081199499, -23.73240184472509995 ) ) ;
#5622 = CARTESIAN_POINT ( 'NONE',  ( 2.783069004973551142, 5.408431875071779693, -23.92277630352788975 ) ) ;
#5623 = VERTEX_POINT ( 'NONE', #14998 ) ;
#5624 = CARTESIAN_POINT ( 'NONE',  ( 2.764680872515352661, -9.232963481057844035, 11.36963888406684298 ) ) ;
#5625 = EDGE_CURVE ( 'NONE', #5216, #2895, #3426, .T. ) ;
#5626 = VECTOR ( 'NONE', #1120, 1000.000000000000000 ) ;
#5627 = TOROIDAL_SURFACE ( 'NONE', #6845, 5.899999999999999467, 0.1000000000000010186 ) ;
#5628 = CARTESIAN_POINT ( 'NONE',  ( 0.000000000000000000, 0.000000000000000000, 5.000000000000000000 ) ) ;
#5629 = VERTEX_POINT ( 'NONE', #5546 ) ;
#5630 = FILL_AREA_STYLE_COLOUR ( '', #9484 ) ;
#5631 = VERTEX_POINT ( 'NONE', #10219 ) ;
#5632 = VERTEX_POINT ( 'NONE', #4536 ) ;
#5633 = ORIENTED_EDGE ( 'NONE', *, *, #12845, .T. ) ;
#5634 = CARTESIAN_POINT ( 'NONE',  ( 0.000000000000000000, -5.249430348645662825, -12.98979500319700264 ) ) ;
#5635 = ADVANCED_FACE ( 'NONE', ( #8987 ), #14973, .T. ) ;
#5636 = DIRECTION ( 'NONE',  ( 1.000000000000000000, 0.000000000000000000, 0.000000000000000000 ) ) ;
#5637 = ADVANCED_FACE ( 'NONE', ( #838 ), #768, .T. ) ;
#5638 = CARTESIAN_POINT ( 'NONE',  ( 93.63799900313688340, -2.337932895214617890, -2.000000000000000888 ) ) ;
#5639 = VECTOR ( 'NONE', #14577, 1000.000000000000000 ) ;
#5640 = CIRCLE ( 'NONE', #11259, 9.999999999999994671 ) ;
#5641 = VECTOR ( 'NONE', #2503, 1000.000000000000000 ) ;
#5642 = CARTESIAN_POINT ( 'NONE',  ( -9.203569561072644802E-15, -8.842327429719173182, 11.12243880662610529 ) ) ;
#5643 = VERTEX_POINT ( 'NONE', #13758 ) ;
#5644 = CARTESIAN_POINT ( 'NONE',  ( 0.07186808533286681566, 23.19485392143213431, 10.24630254990524314 ) ) ;
#5645 = DIRECTION ( 'NONE',  ( 0.000000000000000000, 1.224646799147353207E-16, 1.000000000000000000 ) ) ;
#5646 = EDGE_CURVE ( 'NONE', #1055, #15005, #9118, .T. ) ;
#5647 = CIRCLE ( 'NONE', #3665, 0.1000000000000002554 ) ;
#5648 = CARTESIAN_POINT ( 'NONE',  ( 1.394999999999999574, 4.633866840648922292, 27.68468304288260384 ) ) ;
#5649 = EDGE_CURVE ( 'NONE', #1849, #5700, #1221, .T. ) ;
#5650 = EDGE_LOOP ( 'NONE', ( #5180, #3501, #4633, #6543 ) ) ;
#5651 = DIRECTION ( 'NONE',  ( 0.000000000000000000, 0.000000000000000000, 1.000000000000000000 ) ) ;
#5652 = LINE ( 'NONE', #5794, #1607 ) ;
#5653 = EDGE_CURVE ( 'NONE', #2383, #14287, #7604, .T. ) ;
#5654 = ORIENTED_EDGE ( 'NONE', *, *, #3088, .T. ) ;
#5655 = EDGE_LOOP ( 'NONE', ( #15193, #6229, #4112, #13043, #288, #4030, #2666, #12822 ) ) ;
#5656 = DIRECTION ( 'NONE',  ( 0.000000000000000000, 0.000000000000000000, 1.000000000000000000 ) ) ;
#5657 = AXIS2_PLACEMENT_3D ( 'NONE', #10678, #2227, #1147 ) ;
#5658 = EDGE_CURVE ( 'NONE', #393, #8452, #6370, .T. ) ;
#5659 = ORIENTED_EDGE ( 'NONE', *, *, #5735, .T. ) ;
#5660 = LINE ( 'NONE', #4806, #12213 ) ;
#5661 = FACE_OUTER_BOUND ( 'NONE', #7952, .T. ) ;
#5662 = CARTESIAN_POINT ( 'NONE',  ( 98.48580539929344013, 0.9022481406819604643, 2.999999999999999112 ) ) ;
#5663 = ORIENTED_EDGE ( 'NONE', *, *, #10042, .F. ) ;
#5664 = DIRECTION ( 'NONE',  ( 0.000000000000000000, 0.000000000000000000, 1.000000000000000000 ) ) ;
#5665 = EDGE_LOOP ( 'NONE', ( #1498, #11549, #13230, #1950, #72, #11784 ) ) ;
#5666 = VERTEX_POINT ( 'NONE', #3300 ) ;
#5667 = DIRECTION ( 'NONE',  ( 0.000000000000000000, 0.000000000000000000, 1.000000000000000000 ) ) ;
#5668 = DIRECTION ( 'NONE',  ( -0.000000000000000000, -0.000000000000000000, -1.000000000000000000 ) ) ;
#5669 = DIRECTION ( 'NONE',  ( 0.000000000000000000, 0.000000000000000000, -1.000000000000000000 ) ) ;
#5670 = DIRECTION ( 'NONE',  ( 0.02857142857142857054, -0.9995917534020515305, 0.000000000000000000 ) ) ;
#5671 = B_SPLINE_CURVE_WITH_KNOTS ( 'NONE', 3,
 ( #15116, #12786, #8039, #2272 ),
 .UNSPECIFIED., .F., .F.,
 ( 4, 4 ),
 ( 2.034713381942770033E-07, 0.0006887909409525396235 ),
 .UNSPECIFIED. ) ;
#5672 = CARTESIAN_POINT ( 'NONE',  ( 0.000000000000000000, -7.739906618939614624, -13.40591150984234581 ) ) ;
#5673 = PRODUCT_DEFINITION_SHAPE ( 'NONE', 'NONE',  #11139 ) ;
#5674 = CARTESIAN_POINT ( 'NONE',  ( 2.262072661820534236, -26.82026385750180353, 3.461047254864169975 ) ) ;
#5675 = ORIENTED_EDGE ( 'NONE', *, *, #3534, .T. ) ;
#5676 = CARTESIAN_POINT ( 'NONE',  ( 2.789999999999999147, -7.739906618939802918, 13.40591150984224100 ) ) ;
#5677 = CARTESIAN_POINT ( 'NONE',  ( 2.789999999999999147, 18.28042085475278355, 15.74360496233388140 ) ) ;
#5678 = CARTESIAN_POINT ( 'NONE',  ( -20.63749999999999929, 0.000000000000000000, -4.000000000000000000 ) ) ;
#5679 = ORIENTED_EDGE ( 'NONE', *, *, #14557, .F. ) ;
#5680 =( REPRESENTATION_RELATIONSHIP ('NONE','NONE', #12685, #13067 ) REPRESENTATION_RELATIONSHIP_WITH_TRANSFORMATION ( #12574 )SHAPE_REPRESENTATION_RELATIONSHIP( ) );
#5681 = EDGE_CURVE ( 'NONE', #546, #2234, #7990, .T. ) ;
#5682 = CARTESIAN_POINT ( 'NONE',  ( 1.039999999999997593, 0.000000000000000000, 0.000000000000000000 ) ) ;
#5683 = DIRECTION ( 'NONE',  ( 0.000000000000000000, 0.000000000000000000, 1.000000000000000000 ) ) ;
#5684 = ORIENTED_EDGE ( 'NONE', *, *, #8821, .F. ) ;
#5685 = ORIENTED_EDGE ( 'NONE', *, *, #4325, .T. ) ;
#5686 = DIRECTION ( 'NONE',  ( -1.000000000000000000, -0.000000000000000000, 0.000000000000000000 ) ) ;
#5687 = CARTESIAN_POINT ( 'NONE',  ( 2.765633920072235075, 24.63872515616082737, -2.336989772644355590 ) ) ;
#5688 = VERTEX_POINT ( 'NONE', #12665 ) ;
#5689 = FACE_OUTER_BOUND ( 'NONE', #14024, .T. ) ;
#5690 = CARTESIAN_POINT ( 'NONE',  ( 2.789679245949062913, -20.70663861606260525, -12.51925356660783528 ) ) ;
#5691 = CARTESIAN_POINT ( 'NONE',  ( 2.789999999999999147, -7.909232158574988958, 24.34211360614297348 ) ) ;
#5692 = DIRECTION ( 'NONE',  ( -1.000000000000000000, 0.000000000000000000, 0.000000000000000000 ) ) ;
#5693 = DIRECTION ( 'NONE',  ( -0.000000000000000000, -0.000000000000000000, -1.000000000000000000 ) ) ;
#5694 = EDGE_LOOP ( 'NONE', ( #14539, #8274, #9256, #3628, #6627, #13216 ) ) ;
#5695 = DIRECTION ( 'NONE',  ( -5.480158469902917989E-17, -1.051478716308701742E-16, -1.000000000000000000 ) ) ;
#5696 = B_SPLINE_CURVE_WITH_KNOTS ( 'NONE', 3,
 ( #11699, #5804, #4728, #6949 ),
 .UNSPECIFIED., .F., .F.,
 ( 4, 4 ),
 ( 2.324263106257895883E-07, 0.0006888201370294903293 ),
 .UNSPECIFIED. ) ;
#5697 = CARTESIAN_POINT ( 'NONE',  ( -10.00000000000000000, 0.000000000000000000, 0.000000000000000000 ) ) ;
#5698 = ORIENTED_EDGE ( 'NONE', *, *, #1121, .F. ) ;
#5699 = EDGE_CURVE ( 'NONE', #15019, #14477, #8324, .T. ) ;
#5700 = VERTEX_POINT ( 'NONE', #12451 ) ;
#5701 = ORIENTED_EDGE ( 'NONE', *, *, #2041, .T. ) ;
#5702 = EDGE_LOOP ( 'NONE', ( #8017, #10409, #12030, #9755 ) ) ;
#5703 = CARTESIAN_POINT ( 'NONE',  ( 0.000000000000000000, 0.000000000000000000, 0.000000000000000000 ) ) ;
#5704 = CARTESIAN_POINT ( 'NONE',  ( -14.40394475573012301, -4.794738323547945491, 16.99999999999999645 ) ) ;
#5705 = EDGE_CURVE ( 'NONE', #4548, #5009, #13743, .T. ) ;
#5706 = CARTESIAN_POINT ( 'NONE',  ( 1.039999999999996483, -12.55714665599978375, -12.83329210556844835 ) ) ;
#5707 = CARTESIAN_POINT ( 'NONE',  ( 1.749999999999998002, 0.000000000000000000, 0.000000000000000000 ) ) ;
#5708 = UNCERTAINTY_MEASURE_WITH_UNIT (LENGTH_MEASURE( 1.000000000000000082E-05 ), #13836, 'distance_accuracy_value', 'NONE');
#5709 = CARTESIAN_POINT ( 'NONE',  ( 86.00000000000000000, 7.347880794884117764E-16, 3.000000000000000000 ) ) ;
#5710 = EDGE_LOOP ( 'NONE', ( #8346, #2385, #8381, #11179 ) ) ;
#5711 = CARTESIAN_POINT ( 'NONE',  ( 0.008751532933531189218, -13.40591150985895297, -5.214906618939850524 ) ) ;
#5712 = DIRECTION ( 'NONE',  ( 0.000000000000000000, 0.000000000000000000, 1.000000000000000000 ) ) ;
#5713 = EDGE_CURVE ( 'NONE', #12819, #13750, #3437, .T. ) ;
#5714 = AXIS2_PLACEMENT_3D ( 'NONE', #879, #12331, #10262 ) ;
#5715 = ADVANCED_FACE ( 'NONE', ( #11661 ), #10665, .F. ) ;
#5716 = ORIENTED_EDGE ( 'NONE', *, *, #10856, .T. ) ;
#5717 = DIRECTION ( 'NONE',  ( 0.000000000000000000, 0.000000000000000000, 1.000000000000000000 ) ) ;
#5718 = CARTESIAN_POINT ( 'NONE',  ( 64.00448238961524794, 36.25062540154047497, 5.000000000000000888 ) ) ;
#5719 = ORIENTED_EDGE ( 'NONE', *, *, #4293, .T. ) ;
#5720 = ORIENTED_EDGE ( 'NONE', *, *, #14484, .F. ) ;
#5721 = CIRCLE ( 'NONE', #2985, 2.524999999999997691 ) ;
#5722 = DIRECTION ( 'NONE',  ( -1.000000000000000000, -0.000000000000000000, -0.000000000000000000 ) ) ;
#5723 = ADVANCED_FACE ( 'NONE', ( #4696 ), #10749, .T. ) ;
#5724 = EDGE_CURVE ( 'NONE', #13441, #5629, #5845, .T. ) ;
#5725 = EDGE_LOOP ( 'NONE', ( #3568, #5432, #1320, #3164, #11754, #10810, #6498, #10309 ) ) ;
#5726 = FACE_OUTER_BOUND ( 'NONE', #7587, .T. ) ;
#5727 = LINE ( 'NONE', #9471, #15206 ) ;
#5728 = ADVANCED_FACE ( 'NONE', ( #204 ), #7860, .T. ) ;
#5729 = CARTESIAN_POINT ( 'NONE',  ( 1.039999999999997593, 0.000000000000000000, 0.000000000000000000 ) ) ;
#5730 = DIRECTION ( 'NONE',  ( 1.000000000000000000, 0.000000000000000000, 0.000000000000000000 ) ) ;
#5731 = EDGE_LOOP ( 'NONE', ( #829, #12656, #15159, #10125 ) ) ;
#5732 = FACE_OUTER_BOUND ( 'NONE', #11462, .T. ) ;
#5733 = CARTESIAN_POINT ( 'NONE',  ( 0.7795480803411087845, 4.029281904976870443, -16.99607982911238224 ) ) ;
#5734 = VERTEX_POINT ( 'NONE', #9518 ) ;
#5735 = EDGE_CURVE ( 'NONE', #10191, #7336, #13690, .T. ) ;
#5736 = VERTEX_POINT ( 'NONE', #10448 ) ;
#5737 = SHAPE_REPRESENTATION ( 'hub', ( #1376 ), #12207 ) ;
#5738 = FACE_OUTER_BOUND ( 'NONE', #5063, .T. ) ;
#5739 = DIRECTION ( 'NONE',  ( -1.000000000000000000, 0.000000000000000000, 0.000000000000000000 ) ) ;
#5740 = DIRECTION ( 'NONE',  ( 0.1643989873053574580, -0.9863939238321436376, 0.000000000000000000 ) ) ;
#5741 = DIRECTION ( 'NONE',  ( 0.000000000000000000, 0.000000000000000000, 1.000000000000000000 ) ) ;
#5742 = CARTESIAN_POINT ( 'NONE',  ( 98.48580539929344013, 0.9022481406819604643, 4.000000000000000000 ) ) ;
#5743 = CARTESIAN_POINT ( 'NONE',  ( -4.000000000000000000, 0.000000000000000000, 1.395000000000000462 ) ) ;
#5744 = VERTEX_POINT ( 'NONE', #10530 ) ;
#5745 = CYLINDRICAL_SURFACE ( 'NONE', #7343, 28.06981291497571362 ) ;
#5746 = CARTESIAN_POINT ( 'NONE',  ( -10.00000000000000000, 0.000000000000000000, 0.000000000000000000 ) ) ;
#5747 = CARTESIAN_POINT ( 'NONE',  ( 1.039999999999996705, 19.67366047555530173, 20.02152543075352398 ) ) ;
#5748 = DIRECTION ( 'NONE',  ( 1.000000000000000000, 0.000000000000000000, 0.000000000000000000 ) ) ;
#5749 = EDGE_LOOP ( 'NONE', ( #7088, #1859, #11391, #13531 ) ) ;
#5750 = CARTESIAN_POINT ( 'NONE',  ( 2.789999999999999147, -19.64056340710864745, -14.55412442567638287 ) ) ;
#5751 = CARTESIAN_POINT ( 'NONE',  ( 2.337784068222784839, -15.84984805378628003, -5.191253194756180633 ) ) ;
#5752 = AXIS2_PLACEMENT_3D ( 'NONE', #3953, #7563, #3707 ) ;
#5753 = EDGE_LOOP ( 'NONE', ( #8064, #12484 ) ) ;
#5754 = VECTOR ( 'NONE', #3168, 1000.000000000000000 ) ;
#5755 = ORIENTED_EDGE ( 'NONE', *, *, #10306, .T. ) ;
#5756 = DIRECTION ( 'NONE',  ( 0.000000000000000000, 0.000000000000000000, 1.000000000000000000 ) ) ;
#5757 = CARTESIAN_POINT ( 'NONE',  ( -10.00000000000000000, 0.000000000000000000, 0.000000000000000000 ) ) ;
#5758 = ORIENTED_EDGE ( 'NONE', *, *, #6245, .T. ) ;
#5759 = VECTOR ( 'NONE', #4060, 1000.000000000000000 ) ;
#5760 = DIRECTION ( 'NONE',  ( -1.000000000000000000, -0.000000000000000000, -0.000000000000000000 ) ) ;
#5761 = CARTESIAN_POINT ( 'NONE',  ( 98.63205416320636232, -2.094184955359725375, 2.999999999999999112 ) ) ;
#5762 = CARTESIAN_POINT ( 'NONE',  ( 1.039999999999995373, 12.96210679857822434, -24.89775460606817958 ) ) ;
#5763 = B_SPLINE_CURVE_WITH_KNOTS ( 'NONE', 3,
 ( #12318, #11167, #638, #5573, #9389, #11390 ),
 .UNSPECIFIED., .F., .F.,
 ( 4, 2, 4 ),
 ( 4.462636678184503380E-07, 0.001879885020955184395, 0.003759323778242550443 ),
 .UNSPECIFIED. ) ;
#5764 = DIRECTION ( 'NONE',  ( 0.000000000000000000, 0.000000000000000000, -1.000000000000000000 ) ) ;
#5765 = CARTESIAN_POINT ( 'NONE',  ( 33.82574562093736859, -6.697933970950280091, 2.999999999999999112 ) ) ;
#5766 = CIRCLE ( 'NONE', #8448, 24.12539914357697768 ) ;
#5767 = VERTEX_POINT ( 'NONE', #15145 ) ;
#5768 = DIRECTION ( 'NONE',  ( 0.000000000000000000, 0.000000000000000000, 1.000000000000000000 ) ) ;
#5769 = AXIS2_PLACEMENT_3D ( 'NONE', #7684, #11216, #3232 ) ;
#5770 = CIRCLE ( 'NONE', #6989, 5.000000000000000888 ) ;
#5771 = CARTESIAN_POINT ( 'NONE',  ( 2.789999999999999147, -2.311161484776455222, -14.46287784598619908 ) ) ;
#5772 = EDGE_CURVE ( 'NONE', #5808, #4547, #4840, .T. ) ;
#5773 = ORIENTED_EDGE ( 'NONE', *, *, #14027, .T. ) ;
#5774 = B_SPLINE_CURVE_WITH_KNOTS ( 'NONE', 3,
 ( #8276, #14276, #3668, #12959, #6052, #9296, #2448, #11803 ),
 .UNSPECIFIED., .F., .F.,
 ( 4, 2, 2, 4 ),
 ( 4.663089536307853416E-07, 0.001898630414085407999, 0.002847712466651292768, 0.003796794519217177970 ),
 .UNSPECIFIED. ) ;
#5775 = ORIENTED_EDGE ( 'NONE', *, *, #1254, .T. ) ;
#5776 = ORIENTED_EDGE ( 'NONE', *, *, #5813, .F. ) ;
#5777 = ORIENTED_EDGE ( 'NONE', *, *, #13886, .F. ) ;
#5778 = DIRECTION ( 'NONE',  ( -0.9873505073845697533, 0.1585527532634883052, 0.000000000000000000 ) ) ;
#5779 = AXIS2_PLACEMENT_3D ( 'NONE', #14890, #11414, #3352 ) ;
#5780 = AXIS2_PLACEMENT_3D ( 'NONE', #1089, #13845, #5565 ) ;
#5781 = DIRECTION ( 'NONE',  ( 0.000000000000000000, 0.000000000000000000, 1.000000000000000000 ) ) ;
#5782 = PLANE ( 'NONE',  #11714 ) ;
#5783 = CARTESIAN_POINT ( 'NONE',  ( 0.000000000000000000, 0.000000000000000000, -0.8000000000000000444 ) ) ;
#5784 = EDGE_CURVE ( 'NONE', #1071, #13456, #1406, .T. ) ;
#5785 = DIRECTION ( 'NONE',  ( -1.000000000000000000, -0.000000000000000000, -0.000000000000000000 ) ) ;
#5786 = ADVANCED_FACE ( 'NONE', ( #4623 ), #10597, .T. ) ;
#5787 = ORIENTED_EDGE ( 'NONE', *, *, #10614, .F. ) ;
#5788 = CARTESIAN_POINT ( 'NONE',  ( 80.82762530298222714, -19.99999999999999645, 6.000000000000005329 ) ) ;
#5789 = CIRCLE ( 'NONE', #7249, 28.06981291497571007 ) ;
#5790 = EDGE_CURVE ( 'NONE', #10601, #7097, #12745, .T. ) ;
#5791 = DIRECTION ( 'NONE',  ( 0.000000000000000000, 0.000000000000000000, 1.000000000000000000 ) ) ;
#5792 = ORIENTED_EDGE ( 'NONE', *, *, #14622, .T. ) ;
#5793 = CARTESIAN_POINT ( 'NONE',  ( -10.00000000000000000, -2.081668171172168513E-15, 6.000000000000000000 ) ) ;
#5794 = CARTESIAN_POINT ( 'NONE',  ( 1.394999999999998685, 24.89775460606832524, 12.96210679857795256 ) ) ;
#5795 = VERTEX_POINT ( 'NONE', #6982 ) ;
#5796 = ORIENTED_EDGE ( 'NONE', *, *, #13281, .T. ) ;
#5797 = AXIS2_PLACEMENT_3D ( 'NONE', #8744, #7534, #2694 ) ;
#5798 = ADVANCED_FACE ( 'NONE', ( #3675 ), #8359, .F. ) ;
#5799 = FACE_OUTER_BOUND ( 'NONE', #10338, .T. ) ;
#5800 = B_SPLINE_CURVE_WITH_KNOTS ( 'NONE', 3,
 ( #7555, #12305, #7698, #13300 ),
 .UNSPECIFIED., .F., .F.,
 ( 4, 4 ),
 ( 2.034713381942717623E-07, 0.0006887909409525284563 ),
 .UNSPECIFIED. ) ;
#5801 = ORIENTED_EDGE ( 'NONE', *, *, #9063, .F. ) ;
#5802 = CARTESIAN_POINT ( 'NONE',  ( -14.40394475573012301, -16.79473832354794993, 16.99999999999999645 ) ) ;
#5803 = CARTESIAN_POINT ( 'NONE',  ( 0.02436607992776238310, -2.336989772644097574, -24.63872515616085224 ) ) ;
#5804 = CARTESIAN_POINT ( 'NONE',  ( 2.783025306068356741, 18.43727551351032190, 16.17543236987995314 ) ) ;
#5805 = VECTOR ( 'NONE', #14677, 1000.000000000000000 ) ;
#5806 = CARTESIAN_POINT ( 'NONE',  ( 2.765633920072238183, -5.391175441198789109, 24.15498966839961170 ) ) ;
#5807 = EDGE_CURVE ( 'NONE', #6544, #11663, #7113, .T. ) ;
#5808 = VERTEX_POINT ( 'NONE', #2371 ) ;
#5809 = CIRCLE ( 'NONE', #6041, 17.95481323787947758 ) ;
#5810 = DIRECTION ( 'NONE',  ( -1.000000000000000000, 0.000000000000000000, 0.000000000000000000 ) ) ;
#5811 = DIRECTION ( 'NONE',  ( 1.000000000000000000, 1.445602896647338917E-16, -0.000000000000000000 ) ) ;
#5812 = ORIENTED_EDGE ( 'NONE', *, *, #8796, .F. ) ;
#5813 = EDGE_CURVE ( 'NONE', #15059, #6090, #9433, .T. ) ;
#5814 = VERTEX_POINT ( 'NONE', #8285 ) ;
#5815 = CARTESIAN_POINT ( 'NONE',  ( 0.07181524296601660140, -16.91181672897718968, -18.89296398180210446 ) ) ;
#5816 = DIRECTION ( 'NONE',  ( 1.000000000000000000, 0.000000000000000000, 0.000000000000000000 ) ) ;
#5817 = EDGE_CURVE ( 'NONE', #8792, #9979, #7617, .T. ) ;
#5818 = EDGE_CURVE ( 'NONE', #13731, #555, #11810, .T. ) ;
#5819 = VECTOR ( 'NONE', #3896, 1000.000000000000114 ) ;
#5820 = VECTOR ( 'NONE', #2543, 1000.000000000000000 ) ;
#5821 = FACE_OUTER_BOUND ( 'NONE', #2731, .T. ) ;
#5822 = CARTESIAN_POINT ( 'NONE',  ( -9.403944755730119454, -4.794738323547945491, 12.00000000000000000 ) ) ;
#5823 = ITEM_DEFINED_TRANSFORMATION ( 'NONE', 'NONE', #15076,  #1376 ) ;
#5824 = CYLINDRICAL_SURFACE ( 'NONE', #5873, 8.400000000000000355 ) ;
#5825 = AXIS2_PLACEMENT_3D ( 'NONE', #7307, #11976, #1464 ) ;
#5826 = CARTESIAN_POINT ( 'NONE',  ( 2.715264205769514660, 2.569134216958901984, 15.04916547791955317 ) ) ;
#5827 = VECTOR ( 'NONE', #5811, 1000.000000000000000 ) ;
#5828 = VERTEX_POINT ( 'NONE', #506 ) ;
#5829 = DIRECTION ( 'NONE',  ( -1.000000000000000000, 0.000000000000000000, 0.000000000000000000 ) ) ;
#5830 = CARTESIAN_POINT ( 'NONE',  ( 1.000000000000000000, -5.408326913195983465, 0.000000000000000000 ) ) ;
#5831 = CARTESIAN_POINT ( 'NONE',  ( 60.23740434540291488, 32.40236306526279719, 7.000000000000000000 ) ) ;
#5832 = DIRECTION ( 'NONE',  ( 1.000000000000000000, 0.000000000000000000, 0.000000000000000000 ) ) ;
#5833 = VECTOR ( 'NONE', #15195, 1000.000000000000000 ) ;
#5834 = ORIENTED_EDGE ( 'NONE', *, *, #4250, .F. ) ;
#5835 = ORIENTED_EDGE ( 'NONE', *, *, #7099, .F. ) ;
#5836 = DIRECTION ( 'NONE',  ( -1.000000000000000000, -0.000000000000000000, -0.000000000000000000 ) ) ;
#5837 = ORIENTED_EDGE ( 'NONE', *, *, #5724, .T. ) ;
#5838 = AXIS2_PLACEMENT_3D ( 'NONE', #10962, #13505, #7662 ) ;
#5839 = DIRECTION ( 'NONE',  ( 1.000000000000000000, 0.000000000000000000, -0.000000000000000000 ) ) ;
#5840 = DIRECTION ( 'NONE',  ( 1.000000000000000000, 0.000000000000000000, 0.000000000000000000 ) ) ;
#5841 = EDGE_CURVE ( 'NONE', #8240, #13379, #4925, .T. ) ;
#5842 = CIRCLE ( 'NONE', #6805, 7.000000000000000000 ) ;
#5843 = CARTESIAN_POINT ( 'NONE',  ( 1.394999999999999574, -12.96210679857767900, -24.89775460606846380 ) ) ;
#5844 = CARTESIAN_POINT ( 'NONE',  ( 0.000000000000000000, 23.48180575137729775, 5.535312321042836103 ) ) ;
#5845 = LINE ( 'NONE', #6062, #14236 ) ;
#5846 = DIRECTION ( 'NONE',  ( 1.000000000000000000, 0.000000000000000000, 0.000000000000000000 ) ) ;
#5847 = EDGE_CURVE ( 'NONE', #7404, #5216, #2908, .T. ) ;
#5848 = ORIENTED_EDGE ( 'NONE', *, *, #14084, .F. ) ;
#5849 = AXIS2_PLACEMENT_3D ( 'NONE', #11938, #14028, #4899 ) ;
#5850 = DIRECTION ( 'NONE',  ( 1.000000000000000000, 0.000000000000000000, 0.000000000000000000 ) ) ;
#5851 = VECTOR ( 'NONE', #6614, 1000.000000000000000 ) ;
#5852 = ORIENTED_EDGE ( 'NONE', *, *, #5999, .T. ) ;
#5853 = AXIS2_PLACEMENT_3D ( 'NONE', #13066, #12544, #4255 ) ;
#5854 = CARTESIAN_POINT ( 'NONE',  ( 0.000000000000000000, 0.000000000000000000, 0.000000000000000000 ) ) ;
#5855 = ORIENTED_EDGE ( 'NONE', *, *, #3571, .T. ) ;
#5856 = ORIENTED_EDGE ( 'NONE', *, *, #1020, .F. ) ;
#5857 = VERTEX_POINT ( 'NONE', #11115 ) ;
#5858 = CARTESIAN_POINT ( 'NONE',  ( 0.6538474904312574498, -16.44008199387302582, 5.087730618022520801 ) ) ;
#5859 = CARTESIAN_POINT ( 'NONE',  ( 1.250000000000001110, 0.000000000000000000, 0.000000000000000000 ) ) ;
#5860 = B_SPLINE_CURVE_WITH_KNOTS ( 'NONE', 3,
 ( #7807, #2961, #3199, #11178 ),
 .UNSPECIFIED., .F., .F.,
 ( 4, 4 ),
 ( 2.451234579310841928E-07, 0.0006917187676826554209 ),
 .UNSPECIFIED. ) ;
#5861 = CIRCLE ( 'NONE', #14452, 4.100000000000000533 ) ;
#5862 = CARTESIAN_POINT ( 'NONE',  ( 2.789999999999999147, -15.74360496233368245, -18.28042085475295409 ) ) ;
#5863 = CARTESIAN_POINT ( 'NONE',  ( 67.45386469005195806, 13.93318132202354676, 6.000000000000000000 ) ) ;
#5864 = EDGE_CURVE ( 'NONE', #8779, #2220, #11963, .T. ) ;
#5865 = CARTESIAN_POINT ( 'NONE',  ( 1.749999999999999778, 4.458161950358502601, 17.39253030560843172 ) ) ;
#5866 = CIRCLE ( 'NONE', #14456, 2.999999999999988898 ) ;
#5867 = AXIS2_PLACEMENT_3D ( 'NONE', #7120, #4679, #1206 ) ;
#5868 = ORIENTED_EDGE ( 'NONE', *, *, #9895, .T. ) ;
#5869 = DIRECTION ( 'NONE',  ( 0.000000000000000000, 0.8090169943749400128, 0.5877852522924831291 ) ) ;
#5870 = EDGE_CURVE ( 'NONE', #13727, #12150, #13273, .T. ) ;
#5871 = VECTOR ( 'NONE', #3454, 1000.000000000000000 ) ;
#5872 = VERTEX_POINT ( 'NONE', #1520 ) ;
#5873 = AXIS2_PLACEMENT_3D ( 'NONE', #14031, #9409, #15207 ) ;
#5874 = DIRECTION ( 'NONE',  ( 0.000000000000000000, 0.000000000000000000, 1.000000000000000000 ) ) ;
#5875 = ADVANCED_FACE ( 'NONE', ( #10820 ), #9889, .T. ) ;
#5876 = CARTESIAN_POINT ( 'NONE',  ( 0.02531912748256377743, 14.46287784598617421, -2.311161484776606212 ) ) ;
#5877 = ORIENTED_EDGE ( 'NONE', *, *, #9897, .F. ) ;
#5878 = ORIENTED_EDGE ( 'NONE', *, *, #4984, .T. ) ;
#5879 = CARTESIAN_POINT ( 'NONE',  ( 2.321707774797442170, -4.824281976789052351, 0.000000000000000000 ) ) ;
#5880 = ORIENTED_EDGE ( 'NONE', *, *, #15083, .F. ) ;
#5881 = CARTESIAN_POINT ( 'NONE',  ( 0.000000000000000000, 0.4273491293402468805, -0.8000000000000000444 ) ) ;
#5882 = DIRECTION ( 'NONE',  ( -0.000000000000000000, -0.000000000000000000, -1.000000000000000000 ) ) ;
#5883 = CARTESIAN_POINT ( 'NONE',  ( -14.40394475573011945, -10.79473832354794460, -5.000000000000000000 ) ) ;
#5884 = CARTESIAN_POINT ( 'NONE',  ( 0.000000000000000000, 24.04302995059966719, 1.991882183130389228 ) ) ;
#5885 = B_SPLINE_CURVE_WITH_KNOTS ( 'NONE', 3,
 ( #4576, #3337, #5947, #8027 ),
 .UNSPECIFIED., .F., .F.,
 ( 4, 4 ),
 ( 1.981826382900813409E-07, 0.0006887856082032195850 ),
 .UNSPECIFIED. ) ;
#5886 = ORIENTED_EDGE ( 'NONE', *, *, #4133, .T. ) ;
#5887 = CARTESIAN_POINT ( 'NONE',  ( -14.40394475573011945, -10.79473832354794460, -3.469446951953614189E-15 ) ) ;
#5888 = CARTESIAN_POINT ( 'NONE',  ( -4.000000000000000888, 0.000000000000000000, 10.00000000000000000 ) ) ;
#5889 = EDGE_LOOP ( 'NONE', ( #13203, #9342, #2599, #12409, #781, #11600 ) ) ;
#5890 = ORIENTED_EDGE ( 'NONE', *, *, #9480, .T. ) ;
#5891 = CARTESIAN_POINT ( 'NONE',  ( 0.04999671820202085393, -5.264737421541620499, 13.99876742897257742 ) ) ;
#5892 = AXIS2_PLACEMENT_3D ( 'NONE', #3216, #1907, #7666 ) ;
#5893 = DIRECTION ( 'NONE',  ( 0.000000000000000000, 0.000000000000000000, 1.000000000000000000 ) ) ;
#5894 = EDGE_CURVE ( 'NONE', #7956, #14052, #8592, .T. ) ;
#5895 = CARTESIAN_POINT ( 'NONE',  ( 91.12964445316929130, 15.08873975234342701, -2.000000000000000888 ) ) ;
#5896 = DIRECTION ( 'NONE',  ( 0.000000000000000000, 0.000000000000000000, 1.000000000000000000 ) ) ;
#5897 = LINE ( 'NONE', #14106, #3904 ) ;
#5898 = CARTESIAN_POINT ( 'NONE',  ( 13.78117670802322259, -24.07785181381190753, -2.000000000000000000 ) ) ;
#5899 = ORIENTED_EDGE ( 'NONE', *, *, #9777, .F. ) ;
#5900 = FACE_OUTER_BOUND ( 'NONE', #13110, .T. ) ;
#5901 = FACE_OUTER_BOUND ( 'NONE', #2871, .T. ) ;
#5902 = CARTESIAN_POINT ( 'NONE',  ( -1.033036732025934469E-14, 5.211150952915363455, 13.21889893246977543 ) ) ;
#5903 = AXIS2_PLACEMENT_3D ( 'NONE', #582, #3981, #356 ) ;
#5904 = CARTESIAN_POINT ( 'NONE',  ( 2.790000000000000924, 0.000000000000000000, 4.000000000000000000 ) ) ;
#5905 = ADVANCED_FACE ( 'NONE', ( #431 ), #277, .T. ) ;
#5906 = EDGE_CURVE ( 'NONE', #3044, #5828, #477, .T. ) ;
#5907 = ADVANCED_FACE ( 'NONE', ( #7446 ), #9826, .F. ) ;
#5908 = ORIENTED_EDGE ( 'NONE', *, *, #12475, .F. ) ;
#5909 = ORIENTED_EDGE ( 'NONE', *, *, #6665, .F. ) ;
#5910 = CARTESIAN_POINT ( 'NONE',  ( 0.02436607992775978102, 24.63872515616082737, 2.336989772644355146 ) ) ;
#5911 = EDGE_LOOP ( 'NONE', ( #12756, #3225, #8899, #4684 ) ) ;
#5912 = LINE ( 'NONE', #3444, #1900 ) ;
#5913 = LINE ( 'NONE', #4755, #2398 ) ;
#5914 = CARTESIAN_POINT ( 'NONE',  ( 0.9041604898882313890, 4.928563447326288482, 17.01651022436365324 ) ) ;
#5915 = DIRECTION ( 'NONE',  ( 0.000000000000000000, 0.000000000000000000, 1.000000000000000000 ) ) ;
#5916 = DIRECTION ( 'NONE',  ( -1.000000000000000000, -0.000000000000000000, -0.000000000000000000 ) ) ;
#5917 = CARTESIAN_POINT ( 'NONE',  ( 0.5279273381794601372, -26.82026385750175734, -3.461047254864539457 ) ) ;
#5918 = DIRECTION ( 'NONE',  ( -1.000000000000000000, -0.000000000000000000, -0.000000000000000000 ) ) ;
#5919 = EDGE_CURVE ( 'NONE', #13214, #1249, #12112, .T. ) ;
#5920 = EDGE_CURVE ( 'NONE', #14821, #6969, #3240, .T. ) ;
#5921 = ORIENTED_EDGE ( 'NONE', *, *, #10686, .T. ) ;
#5922 = FACE_OUTER_BOUND ( 'NONE', #10474, .T. ) ;
#5923 = CARTESIAN_POINT ( 'NONE',  ( -19.40394475573012301, -13.79473832354794993, 16.99999999999999645 ) ) ;
#5924 = EDGE_CURVE ( 'NONE', #3172, #3460, #226, .T. ) ;
#5925 = EDGE_LOOP ( 'NONE', ( #14222, #13608, #11895, #6031, #3983, #14498 ) ) ;
#5926 = ORIENTED_EDGE ( 'NONE', *, *, #2132, .T. ) ;
#5927 = ORIENTED_EDGE ( 'NONE', *, *, #9364, .T. ) ;
#5928 = ORIENTED_EDGE ( 'NONE', *, *, #14613, .F. ) ;
#5929 = DIRECTION ( 'NONE',  ( -1.000000000000000000, 0.000000000000000000, -0.000000000000000000 ) ) ;
#5930 = FACE_OUTER_BOUND ( 'NONE', #8748, .T. ) ;
#5931 = ADVANCED_FACE ( 'NONE', ( #1752 ), #6434, .T. ) ;
#5932 = DIRECTION ( 'NONE',  ( 1.000000000000000000, 0.000000000000000000, 0.000000000000000000 ) ) ;
#5933 = LINE ( 'NONE', #5013, #2319 ) ;
#5934 = CARTESIAN_POINT ( 'NONE',  ( 0.02531912748631078014, -2.311161484776655950, 14.46287784598616355 ) ) ;
#5935 = VERTEX_POINT ( 'NONE', #8510 ) ;
#5936 = LINE ( 'NONE', #3693, #1886 ) ;
#5937 = ORIENTED_EDGE ( 'NONE', *, *, #5841, .T. ) ;
#5938 = LINE ( 'NONE', #8233, #2584 ) ;
#5939 = CARTESIAN_POINT ( 'NONE',  ( 2.789999999999999147, 9.836394144775706394, 22.71065055754456097 ) ) ;
#5940 = VERTEX_POINT ( 'NONE', #13111 ) ;
#5941 = ORIENTED_EDGE ( 'NONE', *, *, #8187, .T. ) ;
#5942 = FACE_OUTER_BOUND ( 'NONE', #10804, .T. ) ;
#5943 = ORIENTED_EDGE ( 'NONE', *, *, #2401, .T. ) ;
#5944 = AXIS2_PLACEMENT_3D ( 'NONE', #9284, #11646, #3435 ) ;
#5945 = CARTESIAN_POINT ( 'NONE',  ( 0.007349531976027577629, 14.24968354755768729, 2.217353748341981401 ) ) ;
#5946 = DIRECTION ( 'NONE',  ( -0.000000000000000000, -0.000000000000000000, -1.000000000000000000 ) ) ;
#5947 = CARTESIAN_POINT ( 'NONE',  ( 2.790000000000077307, 23.69897269326684963, -5.456611084821608948 ) ) ;
#5948 = DIRECTION ( 'NONE',  ( 1.000000000000000000, 0.000000000000000000, 0.000000000000000000 ) ) ;
#5949 = VERTEX_POINT ( 'NONE', #2600 ) ;
#5950 = DIRECTION ( 'NONE',  ( 0.000000000000000000, 0.000000000000000000, 1.000000000000000000 ) ) ;
#5951 = CARTESIAN_POINT ( 'NONE',  ( 2.030753610301984313, -19.86438386685646762, -19.12676442129367516 ) ) ;
#5952 = ORIENTED_EDGE ( 'NONE', *, *, #1290, .F. ) ;
#5953 = AXIS2_PLACEMENT_3D ( 'NONE', #943, #12395, #10321 ) ;
#5954 = B_SPLINE_CURVE_WITH_KNOTS ( 'NONE', 3,
 ( #9699, #9546, #14239, #3547, #2634, #3698 ),
 .UNSPECIFIED., .F., .F.,
 ( 4, 2, 4 ),
 ( 4.462636882235905044E-07, 0.001879885203074807597, 0.003759324142461391294 ),
 .UNSPECIFIED. ) ;
#5955 = ORIENTED_EDGE ( 'NONE', *, *, #9652, .T. ) ;
#5956 = CARTESIAN_POINT ( 'NONE',  ( 58.14665764790533586, -0.9105996816177489572, -2.000000000000000888 ) ) ;
#5957 = CARTESIAN_POINT ( 'NONE',  ( -19.40394475573012301, -16.79473832354794993, 12.00000000000000000 ) ) ;
#5958 = LINE ( 'NONE', #8403, #2649 ) ;
#5959 = FACE_OUTER_BOUND ( 'NONE', #11800, .T. ) ;
#5960 = LINE ( 'NONE', #10506, #7834 ) ;
#5961 = LINE ( 'NONE', #8186, #14738 ) ;
#5962 = EDGE_CURVE ( 'NONE', #7105, #3945, #1227, .T. ) ;
#5963 = VERTEX_POINT ( 'NONE', #7376 ) ;
#5964 = CARTESIAN_POINT ( 'NONE',  ( -1.250000000000000666, 5.575000000000000178, 0.000000000000000000 ) ) ;
#5965 = DIRECTION ( 'NONE',  ( 1.000000000000000000, 0.000000000000000000, 0.000000000000000000 ) ) ;
#5966 = DIRECTION ( 'NONE',  ( -1.000000000000000000, 0.000000000000000000, 0.000000000000000000 ) ) ;
#5967 = DIRECTION ( 'NONE',  ( -0.000000000000000000, 0.000000000000000000, 1.000000000000000000 ) ) ;
#5968 = VERTEX_POINT ( 'NONE', #3912 ) ;
#5969 = ADVANCED_FACE ( 'NONE', ( #7291 ), #7900, .F. ) ;
#5970 = ORIENTED_EDGE ( 'NONE', *, *, #13137, .F. ) ;
#5971 = ORIENTED_EDGE ( 'NONE', *, *, #14214, .F. ) ;
#5972 = B_SPLINE_CURVE_WITH_KNOTS ( 'NONE', 3,
 ( #2075, #11443, #4468, #11301, #2157, #6843, #13600, #14841 ),
 .UNSPECIFIED., .F., .F.,
 ( 4, 2, 2, 4 ),
 ( 4.663089413084687740E-07, 0.001898630173449139926, 0.002847712105703055756, 0.003796794037956971370 ),
 .UNSPECIFIED. ) ;
#5973 = CYLINDRICAL_SURFACE ( 'NONE', #13699, 3.000000000000002665 ) ;
#5974 = CARTESIAN_POINT ( 'NONE',  ( -17.10144940350364706, -13.74829019802725050, -3.467067902615131620E-15 ) ) ;
#5975 = CARTESIAN_POINT ( 'NONE',  ( 2.764680872515353105, 13.68080036884348516, 5.229914364928400339 ) ) ;
#5976 = DIRECTION ( 'NONE',  ( 1.000000000000000000, 0.000000000000000000, 0.000000000000000000 ) ) ;
#5977 = DIRECTION ( 'NONE',  ( -0.000000000000000000, -0.000000000000000000, 1.000000000000000000 ) ) ;
#5978 = ADVANCED_FACE ( 'NONE', ( #1824 ), #8885, .F. ) ;
#5979 = EDGE_CURVE ( 'NONE', #6129, #1278, #9814, .T. ) ;
#5980 = EDGE_LOOP ( 'NONE', ( #5214, #14704, #1098, #6527, #1808 ) ) ;
#5981 = DIRECTION ( 'NONE',  ( 0.000000000000000000, -0.000000000000000000, 1.000000000000000000 ) ) ;
#5982 = EDGE_LOOP ( 'NONE', ( #10636, #13358, #8216, #9403 ) ) ;
#5983 = ORIENTED_EDGE ( 'NONE', *, *, #5433, .F. ) ;
#5984 = CARTESIAN_POINT ( 'NONE',  ( 2.321707774797442170, -4.824281976789052351, 0.000000000000000000 ) ) ;
#5985 = FACE_OUTER_BOUND ( 'NONE', #8560, .T. ) ;
#5986 = CARTESIAN_POINT ( 'NONE',  ( 19.20634328910001543, -26.21503864878155099, 4.000000000000000000 ) ) ;
#5987 = ORIENTED_EDGE ( 'NONE', *, *, #5331, .F. ) ;
#5988 = SURFACE_STYLE_USAGE ( .BOTH. , #2302 ) ;
#5989 = AXIS2_PLACEMENT_3D ( 'NONE', #9554, #4881, #1252 ) ;
#5990 = EDGE_LOOP ( 'NONE', ( #9704, #14716, #1978, #8144, #8296, #9390, #12535 ) ) ;
#5991 = ORIENTED_EDGE ( 'NONE', *, *, #6365, .F. ) ;
#5992 = ORIENTED_EDGE ( 'NONE', *, *, #12297, .T. ) ;
#5993 = FACE_OUTER_BOUND ( 'NONE', #11433, .T. ) ;
#5994 = EDGE_CURVE ( 'NONE', #3142, #5499, #4183, .T. ) ;
#5995 = LINE ( 'NONE', #8220, #1440 ) ;
#5996 = CARTESIAN_POINT ( 'NONE',  ( 2.764680872515351773, 11.36963888406687317, 9.232963481057801403 ) ) ;
#5997 = CARTESIAN_POINT ( 'NONE',  ( -9.999999999999998224, -1.390791565672605534, 7.000000000000000000 ) ) ;
#5998 = EDGE_CURVE ( 'NONE', #12499, #393, #6910, .T. ) ;
#5999 = EDGE_CURVE ( 'NONE', #14273, #11143, #13495, .T. ) ;
#6000 = VECTOR ( 'NONE', #10631, 1000.000000000000000 ) ;
#6002 = CIRCLE ( 'NONE', #14597, 0.5999999999999998668 ) ;
#6001 = LINE ( 'NONE', #15167, #7848 ) ;
#6003 = ORIENTED_EDGE ( 'NONE', *, *, #8807, .T. ) ;
#6004 = B_SPLINE_CURVE_WITH_KNOTS ( 'NONE', 3,
 ( #2358, #15130, #11796, #9286 ),
 .UNSPECIFIED., .F., .F.,
 ( 4, 4 ),
 ( 0.005258110598983630792, 0.005948376585272738271 ),
 .UNSPECIFIED. ) ;
#6005 = LINE ( 'NONE', #7160, #14903 ) ;
#6006 = ADVANCED_FACE ( 'NONE', ( #6599, #5383 ), #6512, .F. ) ;
#6007 = VECTOR ( 'NONE', #2275, 1000.000000000000000 ) ;
#6008 = CIRCLE ( 'NONE', #14609, 2.524999999999996358 ) ;
#6009 = VECTOR ( 'NONE', #5201, 1000.000000000000000 ) ;
#6010 = ORIENTED_EDGE ( 'NONE', *, *, #12351, .F. ) ;
#6011 = CARTESIAN_POINT ( 'NONE',  ( 0.000000000000000000, 13.40591150984237245, -7.739906618939567551 ) ) ;
#6012 = CARTESIAN_POINT ( 'NONE',  ( 0.2818303916520938368, -15.25429862889478194, -5.259531939870360162 ) ) ;
#6013 = EDGE_LOOP ( 'NONE', ( #4207, #3899, #11599, #7553 ) ) ;
#6014 = ORIENTED_EDGE ( 'NONE', *, *, #9193, .T. ) ;
#6015 = EDGE_CURVE ( 'NONE', #9599, #9731, #12695, .T. ) ;
#6016 = CARTESIAN_POINT ( 'NONE',  ( 18.21994936526786901, -20.29667510578869027, 7.000000000000000000 ) ) ;
#6017 = ORIENTED_EDGE ( 'NONE', *, *, #795, .T. ) ;
#6018 = CIRCLE ( 'NONE', #12873, 3.799999999999999378 ) ;
#6019 = DIRECTION ( 'NONE',  ( 1.000000000000000000, 0.000000000000000000, 0.000000000000000000 ) ) ;
#6020 = CARTESIAN_POINT ( 'NONE',  ( 2.765633920072242624, -22.71065055754459650, 9.836394144775621129 ) ) ;
#6021 = ADVANCED_FACE ( 'NONE', ( #750 ), #5451, .F. ) ;
#6022 = CARTESIAN_POINT ( 'NONE',  ( -1.150000000000000577, 0.000000000000000000, -5.899999999999999467 ) ) ;
#6023 = CARTESIAN_POINT ( 'NONE',  ( 2.765633920072239516, -24.15498966839958683, -5.391175441198872598 ) ) ;
#6024 = VERTEX_POINT ( 'NONE', #892 ) ;
#6025 = DIRECTION ( 'NONE',  ( 0.000000000000000000, 0.000000000000000000, 1.000000000000000000 ) ) ;
#6026 = CARTESIAN_POINT ( 'NONE',  ( 0.07473579423048559711, 2.569134216959106265, -15.04916547791951764 ) ) ;
#6027 = VERTEX_POINT ( 'NONE', #13656 ) ;
#6028 = CARTESIAN_POINT ( 'NONE',  ( 0.007349505829628596824, -13.44926448535269792, 5.204557061642240079 ) ) ;
#6029 = VECTOR ( 'NONE', #9918, 1000.000000000000000 ) ;
#6030 = VERTEX_POINT ( 'NONE', #3140 ) ;
#6031 = ORIENTED_EDGE ( 'NONE', *, *, #6307, .F. ) ;
#6032 = DIRECTION ( 'NONE',  ( -0.000000000000000000, -0.000000000000000000, 1.000000000000000000 ) ) ;
#6033 = DIRECTION ( 'NONE',  ( -0.9148936170212769170, -0.4036950204470262649, 0.000000000000000000 ) ) ;
#6034 = CARTESIAN_POINT ( 'NONE',  ( 2.790000000000076419, 9.515416771311512534, -22.38018801136466251 ) ) ;
#6035 = CARTESIAN_POINT ( 'NONE',  ( 0.000000000000000000, -7.909232158574647009, -24.34211360614308006 ) ) ;
#6036 = CARTESIAN_POINT ( 'NONE',  ( 1.749999999999999778, 0.000000000000000000, 0.000000000000000000 ) ) ;
#6037 = PRODUCT_DEFINITION_SHAPE ( 'NONE', 'NONE',  #15235 ) ;
#6038 = ADVANCED_FACE ( 'NONE', ( #9127 ), #6817, .T. ) ;
#6039 = CARTESIAN_POINT ( 'NONE',  ( -14.40394475573011945, -10.79473832354794460, 0.7999999999999960476 ) ) ;
#6040 = B_SPLINE_CURVE_WITH_KNOTS ( 'NONE', 3,
 ( #1652, #5276, #14939, #8002 ),
 .UNSPECIFIED., .F., .F.,
 ( 4, 4 ),
 ( 0.005258105385878676132, 0.005948373736081387537 ),
 .UNSPECIFIED. ) ;
#6041 = AXIS2_PLACEMENT_3D ( 'NONE', #8743, #12285, #1759 ) ;
#6042 = VERTEX_POINT ( 'NONE', #816 ) ;
#6043 = DIRECTION ( 'NONE',  ( -1.000000000000000000, 0.000000000000000000, 0.000000000000000000 ) ) ;
#6044 = DIRECTION ( 'NONE',  ( -1.000000000000000000, 0.000000000000000000, -0.000000000000000000 ) ) ;
#6045 = DIRECTION ( 'NONE',  ( 1.000000000000000000, 0.000000000000000000, 0.000000000000000000 ) ) ;
#6046 = DIRECTION ( 'NONE',  ( -1.000000000000000000, -0.000000000000000000, -0.000000000000000000 ) ) ;
#6047 = EDGE_LOOP ( 'NONE', ( #9676, #10865, #2341, #1976 ) ) ;
#6048 = ORIENTED_EDGE ( 'NONE', *, *, #364, .T. ) ;
#6049 = EDGE_CURVE ( 'NONE', #852, #7933, #7259, .T. ) ;
#6050 = TOROIDAL_SURFACE ( 'NONE', #13650, 14.01039946648073986, 8.000000000000000000 ) ;
#6051 = ORIENTED_EDGE ( 'NONE', *, *, #4622, .T. ) ;
#6052 = CARTESIAN_POINT ( 'NONE',  ( 0.2076372544708497692, 10.30022894898806207, 12.04200105039474167 ) ) ;
#6053 = AXIS2_PLACEMENT_3D ( 'NONE', #5356, #8701, #13479 ) ;
#6054 = CARTESIAN_POINT ( 'NONE',  ( 0.000000000000000000, 0.000000000000000000, 5.500000000000000000 ) ) ;
#6055 = EDGE_CURVE ( 'NONE', #8659, #5354, #10199, .T. ) ;
#6056 = CARTESIAN_POINT ( 'NONE',  ( 0.1920564340659374758, 5.295083827234713603, 14.93837896275551813 ) ) ;
#6057 = CIRCLE ( 'NONE', #11930, 6.000000000000001776 ) ;
#6058 = LINE ( 'NONE', #11740, #2814 ) ;
#6059 = CARTESIAN_POINT ( 'NONE',  ( 14.40394475573011945, -10.79473832354794460, -3.200000000000008615 ) ) ;
#6060 = DIRECTION ( 'NONE',  ( 1.000000000000000000, 0.000000000000000000, 0.000000000000000000 ) ) ;
#6061 = ORIENTED_EDGE ( 'NONE', *, *, #4035, .T. ) ;
#6062 = CARTESIAN_POINT ( 'NONE',  ( 3.160591952521659032, -3.281206521718069258, -0.8000000000000000444 ) ) ;
#6063 = DIRECTION ( 'NONE',  ( 0.000000000000000000, 0.000000000000000000, -1.000000000000000000 ) ) ;
#6064 = VERTEX_POINT ( 'NONE', #13578 ) ;
#6065 = DIRECTION ( 'NONE',  ( -1.000000000000000000, -0.000000000000000000, -0.000000000000000000 ) ) ;
#6066 = DIRECTION ( 'NONE',  ( -1.000000000000000000, -0.000000000000000000, -0.000000000000000000 ) ) ;
#6067 = ORIENTED_EDGE ( 'NONE', *, *, #6769, .F. ) ;
#6068 = CIRCLE ( 'NONE', #8029, 2.524999999999995470 ) ;
#6069 = CIRCLE ( 'NONE', #7550, 4.000000000000000888 ) ;
#6070 = ADVANCED_FACE ( 'NONE', ( #11498, #5301 ), #2978, .F. ) ;
#6071 = VECTOR ( 'NONE', #372, 1000.000000000000000 ) ;
#6072 = ORIENTED_EDGE ( 'NONE', *, *, #6135, .F. ) ;
#6073 = ORIENTED_EDGE ( 'NONE', *, *, #7802, .T. ) ;
#6074 = ORIENTED_EDGE ( 'NONE', *, *, #8709, .T. ) ;
#6075 = CARTESIAN_POINT ( 'NONE',  ( 1.039999999999998925, -17.29145405592692342, 4.835383649608409939 ) ) ;
#6076 = LINE ( 'NONE', #7392, #12458 ) ;
#6077 = LINE ( 'NONE', #4709, #8290 ) ;
#6078 = DIRECTION ( 'NONE',  ( -1.000000000000000000, 0.000000000000000000, 0.000000000000000000 ) ) ;
#6079 = ADVANCED_FACE ( 'NONE', ( #13739 ), #6739, .T. ) ;
#6080 = AXIS2_PLACEMENT_3D ( 'NONE', #2064, #6754, #908 ) ;
#6081 = CARTESIAN_POINT ( 'NONE',  ( 2.765633920072241292, 18.55949924794916228, -16.37294372382838148 ) ) ;
#6082 = VECTOR ( 'NONE', #1122, 1000.000000000000114 ) ;
#6083 = EDGE_LOOP ( 'NONE', ( #6325, #3222, #2674, #6951 ) ) ;
#6084 = AXIS2_PLACEMENT_3D ( 'NONE', #13421, #2902, #12270 ) ;
#6085 = DIRECTION ( 'NONE',  ( 0.9021244663126475327, 0.4314758942051350465, -1.141265444721583757E-16 ) ) ;
#6086 = VECTOR ( 'NONE', #10089, 1000.000000000000000 ) ;
#6087 = EDGE_CURVE ( 'NONE', #14849, #4961, #5961, .T. ) ;
#6088 = EDGE_CURVE ( 'NONE', #4492, #368, #5258, .T. ) ;
#6089 = VECTOR ( 'NONE', #3761, 1000.000000000000114 ) ;
#6090 = VERTEX_POINT ( 'NONE', #9411 ) ;
#6091 = DIRECTION ( 'NONE',  ( 1.000000000000000000, 0.000000000000000000, 0.000000000000000000 ) ) ;
#6092 = LINE ( 'NONE', #5939, #4562 ) ;
#6093 = ORIENTED_EDGE ( 'NONE', *, *, #5310, .F. ) ;
#6094 = VERTEX_POINT ( 'NONE', #2278 ) ;
#6095 = AXIS2_PLACEMENT_3D ( 'NONE', #280, #509, #10972 ) ;
#6096 = VECTOR ( 'NONE', #326, 1000.000000000000000 ) ;
#6097 = CYLINDRICAL_SURFACE ( 'NONE', #1362, 5.000000000000000888 ) ;
#6098 = ORIENTED_EDGE ( 'NONE', *, *, #4941, .T. ) ;
#6099 = CARTESIAN_POINT ( 'NONE',  ( 1.394999999999999574, 4.835383649608472112, 17.29145405592690565 ) ) ;
#6100 = CARTESIAN_POINT ( 'NONE',  ( 2.697960337741387438, -15.03709480088670070, -2.583706482362191359 ) ) ;
#6101 = EDGE_CURVE ( 'NONE', #11883, #5435, #6167, .T. ) ;
#6102 = EDGE_CURVE ( 'NONE', #14952, #14366, #3575, .T. ) ;
#6103 = CARTESIAN_POINT ( 'NONE',  ( 2.789999999999999147, 2.680914349914567470E-13, -23.06981291497571362 ) ) ;
#6104 = CARTESIAN_POINT ( 'NONE',  ( 2.718131847775120402, -24.78765742476134548, -5.344160105508965586 ) ) ;
#6105 = VECTOR ( 'NONE', #8084, 1000.000000000000000 ) ;
#6106 = VERTEX_POINT ( 'NONE', #1048 ) ;
#6107 = CARTESIAN_POINT ( 'NONE',  ( 72.49759028996471955, 17.18292470770558822, 6.000000000000000000 ) ) ;
#6108 = EDGE_CURVE ( 'NONE', #7234, #1971, #10012, .T. ) ;
#6109 = DIRECTION ( 'NONE',  ( 0.9988110320138940956, 0.04874958797097354857, 0.000000000000000000 ) ) ;
#6110 = VERTEX_POINT ( 'NONE', #6963 ) ;
#6111 = CARTESIAN_POINT ( 'NONE',  ( 2.789999999999999147, -18.28042085475266276, -15.74360496233401996 ) ) ;
#6112 = ORIENTED_EDGE ( 'NONE', *, *, #9224, .F. ) ;
#6113 = ORIENTED_EDGE ( 'NONE', *, *, #12202, .T. ) ;
#6114 = CARTESIAN_POINT ( 'NONE',  ( 0.006974674093433583938, -24.42374957165207405, 2.249040938978413173 ) ) ;
#6115 = PLANE ( 'NONE',  #697 ) ;
#6116 = ADVANCED_FACE ( 'NONE', ( #10346 ), #1476, .T. ) ;
#6117 = DIRECTION ( 'NONE',  ( 1.000000000000000000, 0.000000000000000000, -0.000000000000000000 ) ) ;
#6118 = CARTESIAN_POINT ( 'NONE',  ( 0.1882239080259273667, 5.251266773802727883, -25.40949241676348080 ) ) ;
#6119 = CIRCLE ( 'NONE', #5404, 2.524999999999999467 ) ;
#6120 = DIRECTION ( 'NONE',  ( -0.04874958797097372204, 0.9988110320138942066, 0.000000000000000000 ) ) ;
#6121 = VERTEX_POINT ( 'NONE', #13017 ) ;
#6122 = CARTESIAN_POINT ( 'NONE',  ( 2.010451917295051238, -5.008579424861679286, 16.73367785739755575 ) ) ;
#6123 = CARTESIAN_POINT ( 'NONE',  ( 0.02531912748679520167, -11.36963888406680923, -9.232963481057881339 ) ) ;
#6124 = CARTESIAN_POINT ( 'NONE',  ( 1.249999999999997780, 5.021051876504148371E-16, 4.100000000000000533 ) ) ;
#6125 = FACE_OUTER_BOUND ( 'NONE', #5665, .T. ) ;
#6126 = ORIENTED_EDGE ( 'NONE', *, *, #2150, .T. ) ;
#6127 = AXIS2_PLACEMENT_3D ( 'NONE', #7763, #2152, #6840 ) ;
#6128 = ORIENTED_EDGE ( 'NONE', *, *, #4859, .F. ) ;
#6129 = VERTEX_POINT ( 'NONE', #3500 ) ;
#6130 = CARTESIAN_POINT ( 'NONE',  ( 0.008751532932800723183, 13.40591150984233870, -5.214906618939568084 ) ) ;
#6131 = CARTESIAN_POINT ( 'NONE',  ( -15.94493884710238696, -7.321218896460230496, -3.000000000000000000 ) ) ;
#6132 = LINE ( 'NONE', #5843, #3373 ) ;
#6133 = CARTESIAN_POINT ( 'NONE',  ( 2.697960371751379149, 9.756102650610401383, -11.73065272960052496 ) ) ;
#6134 = DIRECTION ( 'NONE',  ( -0.9873505073845699753, 0.1585527532634881942, -4.130719410875845176E-17 ) ) ;
#6135 = EDGE_CURVE ( 'NONE', #11582, #7330, #12017, .T. ) ;
#6136 = DIRECTION ( 'NONE',  ( 1.000000000000000000, 0.000000000000000000, 0.000000000000000000 ) ) ;
#6137 = ORIENTED_EDGE ( 'NONE', *, *, #3281, .F. ) ;
#6138 = CARTESIAN_POINT ( 'NONE',  ( 2.789999999999999147, -13.68080036884344963, -5.229914364928496262 ) ) ;
#6139 = CARTESIAN_POINT ( 'NONE',  ( 0.02436607992776021470, 21.30679549418649543, -12.59161484032888723 ) ) ;
#6140 = VERTEX_POINT ( 'NONE', #2352 ) ;
#6141 = CYLINDRICAL_SURFACE ( 'NONE', #683, 4.000000000000000000 ) ;
#6142 = DIRECTION ( 'NONE',  ( 1.000000000000000000, -0.000000000000000000, 0.000000000000000000 ) ) ;
#6143 = FACE_OUTER_BOUND ( 'NONE', #3489, .T. ) ;
#6144 = ADVANCED_FACE ( 'NONE', ( #1268, #8263 ), #10645, .T. ) ;
#6145 = ORIENTED_EDGE ( 'NONE', *, *, #3133, .F. ) ;
#6146 = CARTESIAN_POINT ( 'NONE',  ( 0.09203962824861877667, -11.73065272960070260, 9.756102650610195326 ) ) ;
#6147 = ORIENTED_EDGE ( 'NONE', *, *, #10614, .T. ) ;
#6148 = ORIENTED_EDGE ( 'NONE', *, *, #10018, .T. ) ;
#6149 = EDGE_LOOP ( 'NONE', ( #10437, #2631, #12058, #8857 ) ) ;
#6150 = CARTESIAN_POINT ( 'NONE',  ( 4.000000000000000000, 4.898587196589412829E-16, 6.000000000000000000 ) ) ;
#6151 = DIRECTION ( 'NONE',  ( 0.000000000000000000, 0.000000000000000000, -1.000000000000000000 ) ) ;
#6152 = FACE_OUTER_BOUND ( 'NONE', #12485, .T. ) ;
#6153 = FACE_OUTER_BOUND ( 'NONE', #11585, .T. ) ;
#6154 = DIRECTION ( 'NONE',  ( 0.000000000000000000, 0.000000000000000000, -1.000000000000000000 ) ) ;
#6155 = DIRECTION ( 'NONE',  ( -1.000000000000000000, -0.000000000000000000, -0.000000000000000000 ) ) ;
#6156 = VERTEX_POINT ( 'NONE', #5743 ) ;
#6157 = CARTESIAN_POINT ( 'NONE',  ( 2.765633920072236407, -2.336989772644440855, 24.63872515616082026 ) ) ;
#6158 = EDGE_CURVE ( 'NONE', #8579, #13244, #13756, .T. ) ;
#6159 = EDGE_CURVE ( 'NONE', #14461, #6202, #9281, .T. ) ;
#6160 = EDGE_LOOP ( 'NONE', ( #3169, #9891, #14751, #13572, #6628, #11910 ) ) ;
#6161 = ORIENTED_EDGE ( 'NONE', *, *, #8722, .F. ) ;
#6162 = CARTESIAN_POINT ( 'NONE',  ( 0.000000000000000000, 0.000000000000000000, -10.00000000000000000 ) ) ;
#6163 = CARTESIAN_POINT ( 'NONE',  ( -9.999999999999992895, -25.00000000000000000, 7.000000000000000000 ) ) ;
#6164 = ORIENTED_EDGE ( 'NONE', *, *, #15118, .F. ) ;
#6165 = ORIENTED_EDGE ( 'NONE', *, *, #2512, .F. ) ;
#6166 = DIRECTION ( 'NONE',  ( 0.000000000000000000, 0.000000000000000000, 1.000000000000000000 ) ) ;
#6167 = B_SPLINE_CURVE_WITH_KNOTS ( 'NONE', 3,
 ( #7118, #5826, #2435, #8048, #12946, #3657, #13882, #12722 ),
 .UNSPECIFIED., .F., .F.,
 ( 4, 2, 2, 4 ),
 ( 2.154797737777091420E-07, 0.001895231411415143749, 0.002842739377235822817, 0.003790247343056503404 ),
 .UNSPECIFIED. ) ;
#6168 = EDGE_CURVE ( 'NONE', #12699, #10878, #15046, .T. ) ;
#6169 = ADVANCED_FACE ( 'NONE', ( #6892 ), #15208, .F. ) ;
#6170 = VERTEX_POINT ( 'NONE', #5898 ) ;
#6171 = EDGE_CURVE ( 'NONE', #13716, #13491, #8121, .T. ) ;
#6172 = LINE ( 'NONE', #6099, #3078 ) ;
#6173 = CARTESIAN_POINT ( 'NONE',  ( 1.749999999999999778, -17.39253030560838198, -4.458161950358684678 ) ) ;
#6174 = DIRECTION ( 'NONE',  ( 0.000000000000000000, 0.000000000000000000, 1.000000000000000000 ) ) ;
#6175 = EDGE_LOOP ( 'NONE', ( #14093, #5755, #1584, #13044 ) ) ;
#6176 = CARTESIAN_POINT ( 'NONE',  ( 2.601776105308176934, 2.857713464479052057, -25.78859396478524957 ) ) ;
#6177 = DIRECTION ( 'NONE',  ( 0.000000000000000000, 0.000000000000000000, -1.000000000000000000 ) ) ;
#6178 = ORIENTED_EDGE ( 'NONE', *, *, #15096, .T. ) ;
#6179 = CARTESIAN_POINT ( 'NONE',  ( 1.749999999999999778, 0.000000000000000000, 0.000000000000000000 ) ) ;
#6180 = LINE ( 'NONE', #2793, #14854 ) ;
#6181 = ORIENTED_EDGE ( 'NONE', *, *, #13306, .F. ) ;
#6182 = ORIENTED_EDGE ( 'NONE', *, *, #2784, .T. ) ;
#6183 = FILL_AREA_STYLE ('',( #14499 ) ) ;
#6184 = FACE_OUTER_BOUND ( 'NONE', #5570, .T. ) ;
#6185 = EDGE_CURVE ( 'NONE', #484, #3683, #486, .T. ) ;
#6186 = AXIS2_PLACEMENT_3D ( 'NONE', #14899, #12580, #11200 ) ;
#6187 = DIRECTION ( 'NONE',  ( 0.000000000000000000, 0.000000000000000000, 1.000000000000000000 ) ) ;
#6188 = DIRECTION ( 'NONE',  ( 0.000000000000000000, 0.000000000000000000, 1.000000000000000000 ) ) ;
#6189 = LINE ( 'NONE', #11235, #6357 ) ;
#6190 = ADVANCED_FACE ( 'NONE', ( #13178 ), #8571, .F. ) ;
#6191 = CARTESIAN_POINT ( 'NONE',  ( 18.71314632718394222, -23.25585687728512241, -2.000000000000000000 ) ) ;
#6192 = ORIENTED_EDGE ( 'NONE', *, *, #14537, .F. ) ;
#6193 = DIRECTION ( 'NONE',  ( 0.9148936170212768060, 0.4036950204470267645, -0.000000000000000000 ) ) ;
#6194 = B_SPLINE_CURVE_WITH_KNOTS ( 'NONE', 3,
 ( #8238, #7096, #13063, #4800 ),
 .UNSPECIFIED., .F., .F.,
 ( 4, 4 ),
 ( 3.059063720760159520E-07, 0.0006888942284914164422 ),
 .UNSPECIFIED. ) ;
#6195 = CARTESIAN_POINT ( 'NONE',  ( 4.271534284832219323E-17, 3.369532131271296443E-15, 6.999999999999989342 ) ) ;
#6196 = DIRECTION ( 'NONE',  ( 0.000000000000000000, 0.000000000000000000, 1.000000000000000000 ) ) ;
#6197 = LINE ( 'NONE', #14578, #5819 ) ;
#6198 = EDGE_CURVE ( 'NONE', #1136, #2216, #5182, .T. ) ;
#6199 = TOROIDAL_SURFACE ( 'NONE', #2768, 24.12539914357697768, 8.000000000000000000 ) ;
#6200 = AXIS2_PLACEMENT_3D ( 'NONE', #2109, #13566, #7810 ) ;
#6201 = ORIENTED_EDGE ( 'NONE', *, *, #8319, .T. ) ;
#6202 = VERTEX_POINT ( 'NONE', #5053 ) ;
#6203 = ORIENTED_EDGE ( 'NONE', *, *, #14886, .F. ) ;
#6204 = LINE ( 'NONE', #4136, #2158 ) ;
#6205 = CARTESIAN_POINT ( 'NONE',  ( 0.000000000000000000, -1.991882183130475603, 24.04302995059966719 ) ) ;
#6206 = DIRECTION ( 'NONE',  ( -1.000000000000000000, -0.000000000000000000, -0.000000000000000000 ) ) ;
#6207 = DIRECTION ( 'NONE',  ( 0.000000000000000000, 0.000000000000000000, 1.000000000000000000 ) ) ;
#6208 = DIRECTION ( 'NONE',  ( -0.9237280213470682178, -0.3830490080632377725, 0.000000000000000000 ) ) ;
#6209 = CARTESIAN_POINT ( 'NONE',  ( 1.394999999999999574, 19.67366047555530528, 20.02152543075352753 ) ) ;
#6210 = AXIS2_PLACEMENT_3D ( 'NONE', #3562, #8249, #1560 ) ;
#6211 = VERTEX_POINT ( 'NONE', #489 ) ;
#6212 = DIRECTION ( 'NONE',  ( -1.000000000000000000, -0.000000000000000000, 0.000000000000000000 ) ) ;
#6213 = CARTESIAN_POINT ( 'NONE',  ( 1.039999999999997593, 0.000000000000000000, 0.000000000000000000 ) ) ;
#6214 = ORIENTED_EDGE ( 'NONE', *, *, #5364, .F. ) ;
#6215 = CARTESIAN_POINT ( 'NONE',  ( 1.949486339718610296E-19, -22.37986894186666831, -9.514945144208986960 ) ) ;
#6216 = DIRECTION ( 'NONE',  ( -1.000000000000000000, -0.000000000000000000, -0.000000000000000000 ) ) ;
#6217 = CARTESIAN_POINT ( 'NONE',  ( -5.209999999999999964, 0.000000000000000000, 0.000000000000000000 ) ) ;
#6218 = VERTEX_POINT ( 'NONE', #2576 ) ;
#6219 = CARTESIAN_POINT ( 'NONE',  ( 2.597943646031741771, 15.58455734132147974, -2.883512197588947501 ) ) ;
#6220 = DIRECTION ( 'NONE',  ( -1.000000000000000000, 0.000000000000000000, 0.000000000000000000 ) ) ;
#6221 = ORIENTED_EDGE ( 'NONE', *, *, #9541, .T. ) ;
#6222 = VERTEX_POINT ( 'NONE', #14265 ) ;
#6223 = VERTEX_POINT ( 'NONE', #258 ) ;
#6224 = LINE ( 'NONE', #14763, #6071 ) ;
#6225 = CARTESIAN_POINT ( 'NONE',  ( 2.262072706628479590, 18.56460150496938155, 19.66369668717039332 ) ) ;
#6226 = PLANE ( 'NONE',  #7720 ) ;
#6227 = CARTESIAN_POINT ( 'NONE',  ( 0.02531912748605881155, 13.68080036884355621, -5.229914364928207604 ) ) ;
#6228 = ADVANCED_FACE ( 'NONE', ( #7271 ), #1663, .T. ) ;
#6229 = ORIENTED_EDGE ( 'NONE', *, *, #3001, .T. ) ;
#6230 = DIRECTION ( 'NONE',  ( 0.9988110320138940956, 0.04874958797097353469, -0.000000000000000000 ) ) ;
#6231 = EDGE_LOOP ( 'NONE', ( #6128, #1231, #10736, #8232, #465, #5077 ) ) ;
#6232 = ORIENTED_EDGE ( 'NONE', *, *, #4778, .F. ) ;
#6233 = DIRECTION ( 'NONE',  ( -1.576560579138138762E-17, 1.359337748750801608E-17, -1.000000000000000000 ) ) ;
#6234 = EDGE_CURVE ( 'NONE', #12050, #12694, #14180, .T. ) ;
#6235 = FACE_BOUND ( 'NONE', #13768, .T. ) ;
#6236 = ORIENTED_EDGE ( 'NONE', *, *, #5417, .F. ) ;
#6237 = CIRCLE ( 'NONE', #2311, 17.95481323787947403 ) ;
#6238 = CIRCLE ( 'NONE', #3051, 2.524999999999995914 ) ;
#6239 = EDGE_CURVE ( 'NONE', #4813, #10374, #14836, .T. ) ;
#6240 = UNCERTAINTY_MEASURE_WITH_UNIT (LENGTH_MEASURE( 1.000000000000000082E-05 ), #13124, 'distance_accuracy_value', 'NONE');
#6241 = DIRECTION ( 'NONE',  ( -1.000000000000000000, -1.445602896647338917E-16, 0.000000000000000000 ) ) ;
#6242 = ORIENTED_EDGE ( 'NONE', *, *, #13206, .F. ) ;
#6243 = B_SPLINE_CURVE_WITH_KNOTS ( 'NONE', 3,
 ( #14362, #6287, #8426, #14590, #13112, #2601 ),
 .UNSPECIFIED., .F., .F.,
 ( 4, 2, 4 ),
 ( 4.462636882206429356E-07, 0.001879885203074806513, 0.003759324142461392161 ),
 .UNSPECIFIED. ) ;
#6244 = DIRECTION ( 'NONE',  ( 0.000000000000000000, 0.000000000000000000, 1.000000000000000000 ) ) ;
#6245 = EDGE_CURVE ( 'NONE', #383, #10848, #3726, .T. ) ;
#6246 = FACE_OUTER_BOUND ( 'NONE', #5925, .T. ) ;
#6247 = VECTOR ( 'NONE', #14916, 1000.000000000000000 ) ;
#6248 = CARTESIAN_POINT ( 'NONE',  ( 1.039999999999995373, 12.96210679857822434, -24.89775460606817958 ) ) ;
#6249 =( GEOMETRIC_REPRESENTATION_CONTEXT ( 3 ) GLOBAL_UNCERTAINTY_ASSIGNED_CONTEXT ( ( #11534 ) ) GLOBAL_UNIT_ASSIGNED_CONTEXT ( ( #14041, #10436, #7129 ) ) REPRESENTATION_CONTEXT ( 'NONE', 'WORKASPACE' ) );
#6250 = AXIS2_PLACEMENT_3D ( 'NONE', #8516, #1526, #1830 ) ;
#6251 = ORIENTED_EDGE ( 'NONE', *, *, #14650, .F. ) ;
#6252 = DIRECTION ( 'NONE',  ( -1.000000000000000000, -0.000000000000000000, -0.000000000000000000 ) ) ;
#6253 = CARTESIAN_POINT ( 'NONE',  ( 0.02436607992776064838, 12.59161484032912171, 21.30679549418635688 ) ) ;
#6254 = ORIENTED_EDGE ( 'NONE', *, *, #7210, .F. ) ;
#6255 = CARTESIAN_POINT ( 'NONE',  ( -11.52599798030746037, -13.27615371759915242, -3.873810994203807765E-15 ) ) ;
#6256 = EDGE_CURVE ( 'NONE', #2817, #15071, #5134, .T. ) ;
#6257 = LINE ( 'NONE', #8702, #2085 ) ;
#6258 = ORIENTED_EDGE ( 'NONE', *, *, #10613, .F. ) ;
#6259 = ORIENTED_EDGE ( 'NONE', *, *, #993, .T. ) ;
#6261 = DIRECTION ( 'NONE',  ( 0.7383879686198261405, -0.6743761619433820131, -2.080818337223229863E-17 ) ) ;
#6260 = AXIS2_PLACEMENT_3D ( 'NONE', #10275, #5598, #11274 ) ;
#6262 = VECTOR ( 'NONE', #7778, 1000.000000000000000 ) ;
#6263 = CARTESIAN_POINT ( 'NONE',  ( -1.249999999999997558, 0.000000000000000000, -4.599999999999999645 ) ) ;
#6264 = ADVANCED_FACE ( 'NONE', ( #12171 ), #9542, .T. ) ;
#6265 = CARTESIAN_POINT ( 'NONE',  ( 93.34550147531103903, 3.654933296868752457, 2.999999999999999112 ) ) ;
#6266 = ORIENTED_EDGE ( 'NONE', *, *, #4668, .F. ) ;
#6267 = DIRECTION ( 'NONE',  ( -0.4036950204470272086, 0.9148936170212765839, 0.000000000000000000 ) ) ;
#6268 = CYLINDRICAL_SURFACE ( 'NONE', #13049, 4.000000000000000000 ) ;
#6269 = LINE ( 'NONE', #9811, #13473 ) ;
#6270 = TOROIDAL_SURFACE ( 'NONE', #13129, 24.12539914357697768, 8.000000000000000000 ) ;
#6271 = EDGE_CURVE ( 'NONE', #4588, #567, #7323, .T. ) ;
#6272 = AXIS2_PLACEMENT_3D ( 'NONE', #12549, #8013, #5571 ) ;
#6273 = EDGE_LOOP ( 'NONE', ( #12955, #12182, #10329, #10999 ) ) ;
#6274 = ORIENTED_EDGE ( 'NONE', *, *, #3412, .F. ) ;
#6275 = EDGE_CURVE ( 'NONE', #11370, #11374, #458, .T. ) ;
#6276 = ADVANCED_FACE ( 'NONE', ( #7426 ), #186, .F. ) ;
#6277 = ORIENTED_EDGE ( 'NONE', *, *, #1503, .F. ) ;
#6278 = FACE_OUTER_BOUND ( 'NONE', #3384, .T. ) ;
#6279 = CARTESIAN_POINT ( 'NONE',  ( 55.83172393217232354, 8.817765129169439220, 2.999999999999999112 ) ) ;
#6280 = CARTESIAN_POINT ( 'NONE',  ( 2.765633920072239516, -2.336989772644097574, -24.63872515616085224 ) ) ;
#6281 = CARTESIAN_POINT ( 'NONE',  ( 2.789999999999999147, 14.19996452731189152, 4.595504208220079434 ) ) ;
#6282 = DIRECTION ( 'NONE',  ( -3.490495029680531648E-17, 4.316401690988813706E-17, 1.000000000000000000 ) ) ;
#6283 = LINE ( 'NONE', #6209, #7434 ) ;
#6284 = AXIS2_PLACEMENT_3D ( 'NONE', #2921, #5312, #7610 ) ;
#6285 = ORIENTED_EDGE ( 'NONE', *, *, #12595, .T. ) ;
#6286 = DIRECTION ( 'NONE',  ( 0.000000000000000000, 0.000000000000000000, 1.000000000000000000 ) ) ;
#6287 = CARTESIAN_POINT ( 'NONE',  ( 0.7592463834391192101, -12.05220173035421993, -24.80264696524895385 ) ) ;
#6288 = ORIENTED_EDGE ( 'NONE', *, *, #1570, .T. ) ;
#6289 = DIRECTION ( 'NONE',  ( 1.000000000000000000, 0.000000000000000000, 0.000000000000000000 ) ) ;
#6290 = FACE_OUTER_BOUND ( 'NONE', #2937, .T. ) ;
#6291 = ADVANCED_FACE ( 'NONE', ( #4905 ), #12094, .T. ) ;
#6292 = CARTESIAN_POINT ( 'NONE',  ( 2.764680872515354437, 13.68080036884355621, -5.229914364928207604 ) ) ;
#6293 = EDGE_CURVE ( 'NONE', #2630, #9228, #5640, .T. ) ;
#6294 = ORIENTED_EDGE ( 'NONE', *, *, #5328, .T. ) ;
#6295 = CIRCLE ( 'NONE', #12172, 14.01039946648073986 ) ;
#6296 = EDGE_CURVE ( 'NONE', #4224, #8100, #10872, .T. ) ;
#6297 = DIRECTION ( 'NONE',  ( -1.000000000000000000, -0.000000000000000000, -0.000000000000000000 ) ) ;
#6298 = DIRECTION ( 'NONE',  ( 0.000000000000000000, 0.000000000000000000, 1.000000000000000000 ) ) ;
#6299 = ORIENTED_EDGE ( 'NONE', *, *, #711, .T. ) ;
#6300 = ORIENTED_EDGE ( 'NONE', *, *, #8164, .F. ) ;
#6301 = EDGE_LOOP ( 'NONE', ( #11970, #7537, #3059, #9167 ) ) ;
#6302 = LINE ( 'NONE', #598, #1644 ) ;
#6303 = CARTESIAN_POINT ( 'NONE',  ( 0.06555561860988173839, 21.84113606038307509, 12.72236714503170596 ) ) ;
#6304 = DIRECTION ( 'NONE',  ( 0.000000000000000000, 2.061057595219969177E-15, -1.000000000000000000 ) ) ;
#6305 = DIRECTION ( 'NONE',  ( 0.000000000000000000, 0.000000000000000000, 1.000000000000000000 ) ) ;
#6306 = CARTESIAN_POINT ( 'NONE',  ( 2.789999999999999147, 0.000000000000000000, 0.000000000000000000 ) ) ;
#6307 = EDGE_CURVE ( 'NONE', #7052, #11075, #3831, .T. ) ;
#6308 = AXIS2_PLACEMENT_3D ( 'NONE', #4716, #9692, #9383 ) ;
#6309 = CARTESIAN_POINT ( 'NONE',  ( 2.031033479673586939, 19.86422722021340093, -19.12621924769845805 ) ) ;
#6310 = EDGE_LOOP ( 'NONE', ( #4964, #884, #13160, #8922, #12785, #12298 ) ) ;
#6311 = CARTESIAN_POINT ( 'NONE',  ( 0.02436607992776064838, 5.391175441198615914, 24.15498966839965078 ) ) ;
#6312 = VECTOR ( 'NONE', #4529, 1000.000000000000000 ) ;
#6313 = VECTOR ( 'NONE', #15042, 1000.000000000000000 ) ;
#6314 = VECTOR ( 'NONE', #3041, 1000.000000000000114 ) ;
#6315 = ORIENTED_EDGE ( 'NONE', *, *, #1259, .T. ) ;
#6316 = EDGE_LOOP ( 'NONE', ( #7044, #12568, #2325, #10438 ) ) ;
#6317 = CARTESIAN_POINT ( 'NONE',  ( 1.394999999999998685, 12.96210679857822434, -24.89775460606818314 ) ) ;
#6318 = CARTESIAN_POINT ( 'NONE',  ( 2.789679245949062913, -20.70663861606260525, -12.51925356660783528 ) ) ;
#6319 = ORIENTED_EDGE ( 'NONE', *, *, #13904, .F. ) ;
#6320 = CIRCLE ( 'NONE', #9273, 24.12539914357697413 ) ;
#6321 = VECTOR ( 'NONE', #12861, 1000.000000000000000 ) ;
#6322 = VECTOR ( 'NONE', #5379, 1000.000000000000000 ) ;
#6323 = CIRCLE ( 'NONE', #3620, 4.999999999999997335 ) ;
#6324 = FACE_OUTER_BOUND ( 'NONE', #10392, .T. ) ;
#6325 = ORIENTED_EDGE ( 'NONE', *, *, #4509, .T. ) ;
#6326 = CARTESIAN_POINT ( 'NONE',  ( 0.5321745326902588280, 26.83036154824994668, -3.467596033028380376 ) ) ;
#6327 = CARTESIAN_POINT ( 'NONE',  ( -9.403944755730117677, -7.794738323547949044, 14.99999999999999822 ) ) ;
#6328 = CARTESIAN_POINT ( 'NONE',  ( 33.82574562093736148, -6.697933970950280091, 6.000000000000000000 ) ) ;
#6329 = CIRCLE ( 'NONE', #13449, 17.95481323787947403 ) ;
#6330 = FACE_OUTER_BOUND ( 'NONE', #13215, .T. ) ;
#6331 = EDGE_CURVE ( 'NONE', #12699, #10081, #2804, .T. ) ;
#6332 = FACE_OUTER_BOUND ( 'NONE', #14476, .T. ) ;
#6333 = AXIS2_PLACEMENT_3D ( 'NONE', #9046, #5446, #14974 ) ;
#6334 = VERTEX_POINT ( 'NONE', #798 ) ;
#6335 = DIRECTION ( 'NONE',  ( -1.000000000000000000, -0.000000000000000000, -0.000000000000000000 ) ) ;
#6336 = DIRECTION ( 'NONE',  ( -1.000000000000000000, 0.000000000000000000, 0.000000000000000000 ) ) ;
#6337 = EDGE_LOOP ( 'NONE', ( #10001, #22, #15131, #2141 ) ) ;
#6338 = VERTEX_POINT ( 'NONE', #6576 ) ;
#6339 = CARTESIAN_POINT ( 'NONE',  ( 2.789999999999999147, -9.324097380959603498, 22.25075486061734864 ) ) ;
#6340 = LINE ( 'NONE', #8566, #10758 ) ;
#6341 = CARTESIAN_POINT ( 'NONE',  ( 75.68384697807671557, 11.35494834827056110, 4.000000000000000000 ) ) ;
#6342 = CARTESIAN_POINT ( 'NONE',  ( 2.789999999999999147, -8.624777288397723396, -11.04103753892280615 ) ) ;
#6343 = AXIS2_PLACEMENT_3D ( 'NONE', #3114, #15164, #9235 ) ;
#6344 = VECTOR ( 'NONE', #2281, 1000.000000000000000 ) ;
#6345 = ORIENTED_EDGE ( 'NONE', *, *, #5178, .F. ) ;
#6346 = CARTESIAN_POINT ( 'NONE',  ( -9.999999999999992895, -25.00000000000000000, 3.000000000000002665 ) ) ;
#6347 = CARTESIAN_POINT ( 'NONE',  ( 93.63799900313688340, -2.337932895214617890, 2.999999999999999112 ) ) ;
#6348 = CARTESIAN_POINT ( 'NONE',  ( 4.000000000000000000, 4.898587196589412829E-16, 4.500000000000000888 ) ) ;
#6349 = CARTESIAN_POINT ( 'NONE',  ( 2.789999999999999147, 0.2301004812061083760, -24.44424927289185234 ) ) ;
#6350 = ORIENTED_EDGE ( 'NONE', *, *, #46, .T. ) ;
#6351 = VERTEX_POINT ( 'NONE', #11257 ) ;
#6352 = EDGE_CURVE ( 'NONE', #1772, #2383, #5860, .T. ) ;
#6353 = ORIENTED_EDGE ( 'NONE', *, *, #10308, .F. ) ;
#6354 = CIRCLE ( 'NONE', #6606, 2.999999999999975131 ) ;
#6355 = AXIS2_PLACEMENT_3D ( 'NONE', #1638, #12076, #14170 ) ;
#6356 = DIRECTION ( 'NONE',  ( 1.000000000000000000, 0.000000000000000000, 0.000000000000000000 ) ) ;
#6357 = VECTOR ( 'NONE', #4178, 1000.000000000000000 ) ;
#6358 = DIRECTION ( 'NONE',  ( 1.000000000000000000, 0.000000000000000000, 0.000000000000000000 ) ) ;
#6359 = CARTESIAN_POINT ( 'NONE',  ( 2.262072661820536013, -3.461047254864073164, -26.82026385750182129 ) ) ;
#6360 = CARTESIAN_POINT ( 'NONE',  ( 1.749999999999998002, -4.633866840648726004, -27.68468304288263582 ) ) ;
#6361 = PRODUCT_CONTEXT ( 'NONE', #4987, 'mechanical' ) ;
#6362 = CARTESIAN_POINT ( 'NONE',  ( 1.749999999999998002, -20.02152543075360214, 19.67366047555523068 ) ) ;
#6363 = CARTESIAN_POINT ( 'NONE',  ( 0.07186811453410632544, -18.89333555428542155, -16.91241718342019951 ) ) ;
#6364 = CARTESIAN_POINT ( 'NONE',  ( 2.031033467310408014, 12.98167595241057626, -24.32849926382737138 ) ) ;
#6365 = EDGE_CURVE ( 'NONE', #7999, #1061, #327, .T. ) ;
#6366 = VERTEX_POINT ( 'NONE', #13790 ) ;
#6367 = LINE ( 'NONE', #9665, #14698 ) ;
#6368 = ADVANCED_FACE ( 'NONE', ( #733 ), #12258, .T. ) ;
#6369 = DIRECTION ( 'NONE',  ( -1.000000000000000000, -0.000000000000000000, -0.000000000000000000 ) ) ;
#6370 = CIRCLE ( 'NONE', #4174, 2.524999999999999023 ) ;
#6371 = CARTESIAN_POINT ( 'NONE',  ( 70.16198417812034904, 9.730076655429538590, -2.000000000000000888 ) ) ;
#6372 = VERTEX_POINT ( 'NONE', #7650 ) ;
#6373 = CARTESIAN_POINT ( 'NONE',  ( 0.000000000000000000, 4.898587196589412829E-16, -4.000000000000000000 ) ) ;
#6374 = CARTESIAN_POINT ( 'NONE',  ( 79.18363542992865689, -10.13606076167855541, 6.000000000000005329 ) ) ;
#6375 = ORIENTED_EDGE ( 'NONE', *, *, #4779, .T. ) ;
#6376 = ORIENTED_EDGE ( 'NONE', *, *, #2998, .F. ) ;
#6377 = DIRECTION ( 'NONE',  ( -0.9873505073845697533, 0.1585527532634883052, 0.000000000000000000 ) ) ;
#6378 = CARTESIAN_POINT ( 'NONE',  ( 0.8291131470075423504, 24.44424927289185945, 12.96989951879416125 ) ) ;
#6379 = CARTESIAN_POINT ( 'NONE',  ( -0.1374368770859597522, -4.808326913195983821, 0.000000000000000000 ) ) ;
#6380 = CYLINDRICAL_SURFACE ( 'NONE', #4782, 2.524999999999995914 ) ;
#6381 = EDGE_CURVE ( 'NONE', #13727, #7471, #9061, .T. ) ;
#6382 = AXIS2_PLACEMENT_3D ( 'NONE', #11278, #10278, #10054 ) ;
#6383 = DIRECTION ( 'NONE',  ( -1.000000000000000000, 0.000000000000000000, -0.000000000000000000 ) ) ;
#6384 = EDGE_CURVE ( 'NONE', #2971, #6697, #415, .T. ) ;
#6385 = CARTESIAN_POINT ( 'NONE',  ( 10.00000000000000178, -1.390791565672601315, 7.000000000000006217 ) ) ;
#6386 = EDGE_CURVE ( 'NONE', #9357, #6351, #1733, .T. ) ;
#6387 = VERTEX_POINT ( 'NONE', #4430 ) ;
#6388 = PRODUCT ( 'angular contact ball bearing_68_iso_ISO 15 ABB - 178 - 20,SI,NC,20_68', 'angular contact ball bearing_68_iso_ISO 15 ABB - 178 - 20,SI,NC,20_68', '', ( #1821 ) ) ;
#6389 = LINE ( 'NONE', #531, #11627 ) ;
#6390 = B_SPLINE_CURVE_WITH_KNOTS ( 'NONE', 3,
 ( #8977, #10208, #4455, #7752 ),
 .UNSPECIFIED., .F., .F.,
 ( 4, 4 ),
 ( 2.324263106244697256E-07, 0.0006888201370294697295 ),
 .UNSPECIFIED. ) ;
#6391 = EDGE_CURVE ( 'NONE', #2220, #1813, #14472, .T. ) ;
#6392 =( NAMED_UNIT ( * ) SI_UNIT ( $, .STERADIAN. ) SOLID_ANGLE_UNIT ( ) );
#6393 = ORIENTED_EDGE ( 'NONE', *, *, #7511, .F. ) ;
#6394 = ORIENTED_EDGE ( 'NONE', *, *, #3006, .T. ) ;
#6395 = ORIENTED_EDGE ( 'NONE', *, *, #8150, .T. ) ;
#6396 = CARTESIAN_POINT ( 'NONE',  ( -14.40394475573011945, -10.79473832354794460, 0.7999999999999960476 ) ) ;
#6397 = CARTESIAN_POINT ( 'NONE',  ( 2.789999999999999147, 5.535312321043049266, -23.48180575137724446 ) ) ;
#6398 = VERTEX_POINT ( 'NONE', #12492 ) ;
#6399 = PRODUCT_DEFINITION_CONTEXT ( 'detailed design', #3900, 'design' ) ;
#6400 = DIRECTION ( 'NONE',  ( -1.000000000000000000, -0.000000000000000000, -0.000000000000000000 ) ) ;
#6401 = ORIENTED_EDGE ( 'NONE', *, *, #3084, .F. ) ;
#6402 = CARTESIAN_POINT ( 'NONE',  ( 0.07181525068722525995, 25.22524549359950541, -2.576941577947494011 ) ) ;
#6403 = CARTESIAN_POINT ( 'NONE',  ( -20.63749999999999574, 0.000000000000000000, 0.000000000000000000 ) ) ;
#6404 = CARTESIAN_POINT ( 'NONE',  ( 0.1438988480159978933, 14.59528211758547478, 5.279841123860917307 ) ) ;
#6405 = DIRECTION ( 'NONE',  ( 1.000000000000000000, 0.000000000000000000, 0.000000000000000000 ) ) ;
#6406 = FACE_BOUND ( 'NONE', #2095, .T. ) ;
#6407 = ORIENTED_EDGE ( 'NONE', *, *, #7370, .F. ) ;
#6408 = DIRECTION ( 'NONE',  ( -0.000000000000000000, -0.000000000000000000, 1.000000000000000000 ) ) ;
#6409 = LINE ( 'NONE', #8859, #6009 ) ;
#6410 = VERTEX_POINT ( 'NONE', #10032 ) ;
#6411 = ORIENTED_EDGE ( 'NONE', *, *, #5724, .F. ) ;
#6412 = CARTESIAN_POINT ( 'NONE',  ( 0.000000000000000000, 0.000000000000000000, 0.000000000000000000 ) ) ;
#6413 = DIRECTION ( 'NONE',  ( -1.000000000000000000, 0.000000000000000000, 0.000000000000000000 ) ) ;
#6414 = DIRECTION ( 'NONE',  ( 0.000000000000000000, 0.000000000000000000, -1.000000000000000000 ) ) ;
#6415 = DIRECTION ( 'NONE',  ( 0.000000000000000000, 0.000000000000000000, 1.000000000000000000 ) ) ;
#6416 = ADVANCED_FACE ( 'NONE', ( #6653 ), #11397, .F. ) ;
#6417 = ORIENTED_EDGE ( 'NONE', *, *, #6671, .T. ) ;
#6418 = FACE_OUTER_BOUND ( 'NONE', #3065, .T. ) ;
#6419 = DIRECTION ( 'NONE',  ( 0.000000000000000000, 0.000000000000000000, 1.000000000000000000 ) ) ;
#6420 = CARTESIAN_POINT ( 'NONE',  ( 0.02436607992776455150, 21.30679549418631780, 12.59161484032919986 ) ) ;
#6421 =( LENGTH_UNIT ( ) NAMED_UNIT ( * ) SI_UNIT ( .MILLI., .METRE. ) );
#6422 = ORIENTED_EDGE ( 'NONE', *, *, #11479, .T. ) ;
#6423 = ORIENTED_EDGE ( 'NONE', *, *, #6271, .T. ) ;
#6424 = AXIS2_PLACEMENT_3D ( 'NONE', #14194, #14035, #13970 ) ;
#6425 = ORIENTED_EDGE ( 'NONE', *, *, #13988, .T. ) ;
#6426 = CARTESIAN_POINT ( 'NONE',  ( 2.718131864678288601, 2.577209017047007666, 25.22589920183362722 ) ) ;
#6427 = FACE_OUTER_BOUND ( 'NONE', #9120, .T. ) ;
#6428 = ADVANCED_FACE ( 'NONE', ( #14730 ), #875, .T. ) ;
#6429 = FACE_OUTER_BOUND ( 'NONE', #11783, .T. ) ;
#6430 = CYLINDRICAL_SURFACE ( 'NONE', #13365, 8.400000000000000355 ) ;
#6431 = ITEM_DEFINED_TRANSFORMATION ( 'NONE', 'NONE', #11129,  #1376 ) ;
#6432 = FACE_OUTER_BOUND ( 'NONE', #7421, .T. ) ;
#6433 = ADVANCED_FACE ( 'NONE', ( #8797 ), #7882, .F. ) ;
#6434 = PLANE ( 'NONE',  #5903 ) ;
#6435 = CARTESIAN_POINT ( 'NONE',  ( 2.783025336474041822, 12.53640742967753141, 21.08118142846907972 ) ) ;
#6436 = EDGE_LOOP ( 'NONE', ( #6061, #7290, #11123, #6605 ) ) ;
#6437 = CARTESIAN_POINT ( 'NONE',  ( 80.00000000000000000, 0.000000000000000000, 4.000000000000003553 ) ) ;
#6438 = AXIS2_PLACEMENT_3D ( 'NONE', #5662, #10184, #3265 ) ;
#6439 = DIRECTION ( 'NONE',  ( 1.000000000000000000, 0.000000000000000000, 0.000000000000000000 ) ) ;
#6440 = EDGE_CURVE ( 'NONE', #5814, #12657, #7723, .T. ) ;
#6441 = DIRECTION ( 'NONE',  ( -0.000000000000000000, -0.000000000000000000, -1.000000000000000000 ) ) ;
#6442 = B_SPLINE_CURVE_WITH_KNOTS ( 'NONE', 3,
 ( #3427, #8256, #12937, #8115 ),
 .UNSPECIFIED., .F., .F.,
 ( 4, 4 ),
 ( 2.034713381942717888E-07, 0.0006045424356927869836 ),
 .UNSPECIFIED. ) ;
#6443 = ORIENTED_EDGE ( 'NONE', *, *, #13563, .F. ) ;
#6444 = LINE ( 'NONE', #11121, #1141 ) ;
#6445 = DIRECTION ( 'NONE',  ( -0.000000000000000000, -0.000000000000000000, 1.000000000000000000 ) ) ;
#6446 = ORIENTED_EDGE ( 'NONE', *, *, #4470, .T. ) ;
#6447 = ORIENTED_EDGE ( 'NONE', *, *, #12767, .T. ) ;
#6448 =( NAMED_UNIT ( * ) SI_UNIT ( $, .STERADIAN. ) SOLID_ANGLE_UNIT ( ) );
#6449 = DIRECTION ( 'NONE',  ( 0.000000000000000000, 0.000000000000000000, 1.000000000000000000 ) ) ;
#6450 = EDGE_CURVE ( 'NONE', #3757, #14414, #5147, .T. ) ;
#6451 = AXIS2_PLACEMENT_3D ( 'NONE', #5223, #3745, #13109 ) ;
#6452 = EDGE_CURVE ( 'NONE', #6485, #15027, #6323, .T. ) ;
#6453 = CARTESIAN_POINT ( 'NONE',  ( 0.000000000000000000, 5.535312321043032391, -23.48180575137725867 ) ) ;
#6454 = FACE_OUTER_BOUND ( 'NONE', #4584, .T. ) ;
#6455 = CARTESIAN_POINT ( 'NONE',  ( 2.764680872515353993, -5.229914364928256454, -13.68080036884353845 ) ) ;
#6456 = DIRECTION ( 'NONE',  ( -1.000000000000000000, -0.000000000000000000, -0.000000000000000000 ) ) ;
#6457 =( REPRESENTATION_RELATIONSHIP ('NONE','NONE', #12685, #7313 ) REPRESENTATION_RELATIONSHIP_WITH_TRANSFORMATION ( #15205 )SHAPE_REPRESENTATION_RELATIONSHIP( ) );
#6458 = ORIENTED_EDGE ( 'NONE', *, *, #12667, .T. ) ;
#6459 = CARTESIAN_POINT ( 'NONE',  ( -5.209999999999999964, 0.000000000000000000, 0.000000000000000000 ) ) ;
#6460 = CARTESIAN_POINT ( 'NONE',  ( -9.403944755730117677, -16.79473832354794993, 16.99999999999999645 ) ) ;
#6461 = EDGE_CURVE ( 'NONE', #6579, #4703, #8388, .T. ) ;
#6462 = EDGE_LOOP ( 'NONE', ( #11520, #11943, #5359, #7331 ) ) ;
#6463 = ORIENTED_EDGE ( 'NONE', *, *, #8243, .T. ) ;
#6464 = ORIENTED_EDGE ( 'NONE', *, *, #10555, .F. ) ;
#6465 = CYLINDRICAL_SURFACE ( 'NONE', #5555, 13.19999999999999929 ) ;
#6466 = EDGE_CURVE ( 'NONE', #4703, #9629, #8279, .T. ) ;
#6467 = CARTESIAN_POINT ( 'NONE',  ( 0.000000000000000000, 0.000000000000000000, 3.895000000000000462 ) ) ;
#6468 = EDGE_CURVE ( 'NONE', #15110, #9070, #1201, .T. ) ;
#6469 = CARTESIAN_POINT ( 'NONE',  ( -19.40394475573012301, -7.794738323547950820, 14.99999999999999822 ) ) ;
#6470 = CARTESIAN_POINT ( 'NONE',  ( 0.07181524296601550506, -18.89296398180203695, 16.91181672897726784 ) ) ;
#6471 = ORIENTED_EDGE ( 'NONE', *, *, #13221, .T. ) ;
#6472 = DIRECTION ( 'NONE',  ( -1.000000000000000000, -0.000000000000000000, 0.000000000000000000 ) ) ;
#6473 = CARTESIAN_POINT ( 'NONE',  ( 64.00448238961524794, 36.25062540154047497, -8.169391093593850073 ) ) ;
#6474 = AXIS2_PLACEMENT_3D ( 'NONE', #3170, #4296, #5976 ) ;
#6475 = CARTESIAN_POINT ( 'NONE',  ( 2.789999999999999147, -4.595504208219929332, -14.19996452731193948 ) ) ;
#6476 = DIRECTION ( 'NONE',  ( 0.4571871344001383619, 0.8893705212896307888, 0.000000000000000000 ) ) ;
#6477 = CARTESIAN_POINT ( 'NONE',  ( 2.789999999999999147, -20.70663861606260170, -12.51925356660783528 ) ) ;
#6478 = VECTOR ( 'NONE', #13069, 1000.000000000000000 ) ;
#6479 = AXIS2_PLACEMENT_3D ( 'NONE', #3387, #2233, #11445 ) ;
#6480 = ORIENTED_EDGE ( 'NONE', *, *, #7879, .T. ) ;
#6481 = CARTESIAN_POINT ( 'NONE',  ( 2.789999999999999147, 23.31896751603331808, 7.334849878007589474 ) ) ;
#6482 = CARTESIAN_POINT ( 'NONE',  ( -6.158890435332099336E-14, 13.21862218141514234, 5.211197193340741940 ) ) ;
#6483 = VECTOR ( 'NONE', #14522, 1000.000000000000000 ) ;
#6484 = ORIENTED_EDGE ( 'NONE', *, *, #5526, .F. ) ;
#6485 = VERTEX_POINT ( 'NONE', #10400 ) ;
#6486 = CARTESIAN_POINT ( 'NONE',  ( 2.021362740937213687, -5.021526291670196152, -16.74220655292943505 ) ) ;
#6487 = DIRECTION ( 'NONE',  ( 1.000000000000000000, 0.000000000000000000, 0.000000000000000000 ) ) ;
#6488 = DIRECTION ( 'NONE',  ( 1.000000000000000000, 0.000000000000000000, -0.000000000000000000 ) ) ;
#6489 = AXIS2_PLACEMENT_3D ( 'NONE', #11435, #912, #9300 ) ;
#6490 = EDGE_CURVE ( 'NONE', #2553, #13780, #5660, .T. ) ;
#6491 = AXIS2_PLACEMENT_3D ( 'NONE', #11366, #6532, #9143 ) ;
#6492 = CARTESIAN_POINT ( 'NONE',  ( -14.40394475573011768, -16.79473832354794993, 16.99999999999999645 ) ) ;
#6493 = MECHANICAL_DESIGN_GEOMETRIC_PRESENTATION_REPRESENTATION (  '', ( #5037 ), #10913 ) ;
#6494 = B_SPLINE_CURVE_WITH_KNOTS ( 'NONE', 3,
 ( #13292, #13225, #2772, #7465, #13529, #13368 ),
 .UNSPECIFIED., .F., .F.,
 ( 4, 2, 4 ),
 ( 2.586195665736120714E-07, 0.001878649493629692274, 0.003757040367692811213 ),
 .UNSPECIFIED. ) ;
#6495 = ORIENTED_EDGE ( 'NONE', *, *, #12546, .T. ) ;
#6496 = CARTESIAN_POINT ( 'NONE',  ( 1.749999999999998002, 12.52377138324259143, -25.12109765559640451 ) ) ;
#6497 = CARTESIAN_POINT ( 'NONE',  ( 2.789999999999999147, -8.936381166381891568E-14, 25.59481291497571220 ) ) ;
#6498 = ORIENTED_EDGE ( 'NONE', *, *, #7988, .T. ) ;
#6499 = DIRECTION ( 'NONE',  ( -1.000000000000000000, -0.000000000000000000, -0.000000000000000000 ) ) ;
#6500 = ORIENTED_EDGE ( 'NONE', *, *, #14660, .T. ) ;
#6501 = VERTEX_POINT ( 'NONE', #11698 ) ;
#6502 = CIRCLE ( 'NONE', #3552, 9.999999999999994671 ) ;
#6503 = AXIS2_PLACEMENT_3D ( 'NONE', #71, #3771, #9464 ) ;
#6504 = ORIENTED_EDGE ( 'NONE', *, *, #6256, .F. ) ;
#6505 = FILL_AREA_STYLE ('',( #809 ) ) ;
#6506 = CARTESIAN_POINT ( 'NONE',  ( 32.66827876307085887, -1.833751565556681173, 6.000000000000000000 ) ) ;
#6507 = EDGE_CURVE ( 'NONE', #5489, #6410, #1253, .T. ) ;
#6508 = CYLINDRICAL_SURFACE ( 'NONE', #1403, 13.19999999999999929 ) ;
#6509 = DIRECTION ( 'NONE',  ( -0.4055247608874392173, 0.9140840597599245720, -7.389059384413459453E-17 ) ) ;
#6510 = APPLICATION_PROTOCOL_DEFINITION ( 'draft international standard', 'automotive_design', 1998, #2624 ) ;
#6511 = CARTESIAN_POINT ( 'NONE',  ( 0.5537796877189864464, -11.41743294611084103, 12.52687487503415298 ) ) ;
#6512 = PLANE ( 'NONE',  #3196 ) ;
#6513 = DIRECTION ( 'NONE',  ( 1.000000000000000000, 0.000000000000000000, 0.000000000000000000 ) ) ;
#6514 = AXIS2_PLACEMENT_3D ( 'NONE', #3551, #3630, #8320 ) ;
#6515 = ORIENTED_EDGE ( 'NONE', *, *, #4668, .T. ) ;
#6516 = FACE_OUTER_BOUND ( 'NONE', #14994, .T. ) ;
#6517 = AXIS2_PLACEMENT_3D ( 'NONE', #10325, #12837, #2096 ) ;
#6518 = CARTESIAN_POINT ( 'NONE',  ( 1.039999999999996927, 4.835383649608473000, 17.29145405592690565 ) ) ;
#6519 = AXIS2_PLACEMENT_3D ( 'NONE', #8869, #13565, #10183 ) ;
#6520 = CARTESIAN_POINT ( 'NONE',  ( 0.000000000000000000, 0.000000000000000000, 0.000000000000000000 ) ) ;
#6521 = EDGE_CURVE ( 'NONE', #11429, #10552, #5727, .T. ) ;
#6522 = ORIENTED_EDGE ( 'NONE', *, *, #5365, .F. ) ;
#6523 = ADVANCED_FACE ( 'NONE', ( #3263 ), #6797, .F. ) ;
#6524 = FACE_OUTER_BOUND ( 'NONE', #13859, .T. ) ;
#6525 = CYLINDRICAL_SURFACE ( 'NONE', #5797, 8.400000000000000355 ) ;
#6526 = VERTEX_POINT ( 'NONE', #13945 ) ;
#6527 = ORIENTED_EDGE ( 'NONE', *, *, #1527, .T. ) ;
#6528 = VECTOR ( 'NONE', #1715, 1000.000000000000000 ) ;
#6529 = CARTESIAN_POINT ( 'NONE',  ( 1.000000000000000000, -5.408326913195983465, -0.8000000000000000444 ) ) ;
#6530 = DIRECTION ( 'NONE',  ( 0.000000000000000000, 0.000000000000000000, -1.000000000000000000 ) ) ;
#6531 = CARTESIAN_POINT ( 'NONE',  ( 1.039999999999997593, 0.000000000000000000, 0.000000000000000000 ) ) ;
#6532 = DIRECTION ( 'NONE',  ( -1.000000000000000000, -0.000000000000000000, -0.000000000000000000 ) ) ;
#6533 = CARTESIAN_POINT ( 'NONE',  ( 55.83172393217232354, 8.817765129169439220, 7.000000000000000000 ) ) ;
#6534 = CARTESIAN_POINT ( 'NONE',  ( -3.160591952521660364, -3.281206521718067037, 0.000000000000000000 ) ) ;
#6535 = ORIENTED_EDGE ( 'NONE', *, *, #6578, .F. ) ;
#6536 = VECTOR ( 'NONE', #6142, 1000.000000000000000 ) ;
#6537 = DIRECTION ( 'NONE',  ( -0.000000000000000000, -0.000000000000000000, -1.000000000000000000 ) ) ;
#6538 = CIRCLE ( 'NONE', #8742, 0.1000000000000002554 ) ;
#6539 = CARTESIAN_POINT ( 'NONE',  ( -19.40394475573012301, -13.79473832354794993, 14.99999999999999822 ) ) ;
#6540 = VERTEX_POINT ( 'NONE', #15 ) ;
#6541 =( LENGTH_UNIT ( ) NAMED_UNIT ( * ) SI_UNIT ( .MILLI., .METRE. ) );
#6542 = ORIENTED_EDGE ( 'NONE', *, *, #1134, .T. ) ;
#6543 = ORIENTED_EDGE ( 'NONE', *, *, #1569, .F. ) ;
#6544 = VERTEX_POINT ( 'NONE', #1032 ) ;
#6545 = DIRECTION ( 'NONE',  ( 0.000000000000000000, 0.000000000000000000, 1.000000000000000000 ) ) ;
#6546 = CARTESIAN_POINT ( 'NONE',  ( 2.790000000000060876, -14.05326139264726137, -2.096282088614914940 ) ) ;
#6547 = CIRCLE ( 'NONE', #3600, 24.12539914357697413 ) ;
#6548 = EDGE_CURVE ( 'NONE', #3069, #5814, #12062, .T. ) ;
#6549 = AXIS2_PLACEMENT_3D ( 'NONE', #10094, #4260, #8936 ) ;
#6550 = B_SPLINE_CURVE_WITH_KNOTS ( 'NONE', 3,
 ( #10795, #9633, #1495, #8561, #14327, #13168, #2654, #7347 ),
 .UNSPECIFIED., .F., .F.,
 ( 4, 2, 2, 4 ),
 ( 2.445728210282191027E-07, 0.001895260649874687875, 0.002842768688401520541, 0.003790276726928352991 ),
 .UNSPECIFIED. ) ;
#6551 = AXIS2_PLACEMENT_3D ( 'NONE', #518, #14462, #7538 ) ;
#6552 = DIRECTION ( 'NONE',  ( 0.1643989873053580408, -0.9863939238321435266, -0.000000000000000000 ) ) ;
#6553 = CIRCLE ( 'NONE', #15155, 2.524999999999996358 ) ;
#6554 = FACE_OUTER_BOUND ( 'NONE', #5613, .T. ) ;
#6555 = ORIENTED_EDGE ( 'NONE', *, *, #5548, .F. ) ;
#6556 = CYLINDRICAL_SURFACE ( 'NONE', #8695, 4.424999999999999822 ) ;
#6557 = FACE_OUTER_BOUND ( 'NONE', #11286, .T. ) ;
#6558 = EDGE_CURVE ( 'NONE', #10985, #12627, #11481, .T. ) ;
#6559 = EDGE_CURVE ( 'NONE', #188, #3346, #15029, .T. ) ;
#6560 = CARTESIAN_POINT ( 'NONE',  ( 0.1855654851361731306, -10.67816411292181655, 23.63475234378979195 ) ) ;
#6561 = CIRCLE ( 'NONE', #13173, 24.12539914357697768 ) ;
#6562 = CARTESIAN_POINT ( 'NONE',  ( 0.000000000000000000, 0.000000000000000000, 10.00000000000000000 ) ) ;
#6563 = EDGE_LOOP ( 'NONE', ( #13247, #10532, #2174, #1160 ) ) ;
#6564 = VECTOR ( 'NONE', #8201, 999.9999999999998863 ) ;
#6565 = CARTESIAN_POINT ( 'NONE',  ( 1.749999999999999778, 4.835383649608472112, 17.29145405592690210 ) ) ;
#6566 = CARTESIAN_POINT ( 'NONE',  ( 2.021362784118868827, -12.71987259277426574, -11.98841295390611528 ) ) ;
#6567 = CIRCLE ( 'NONE', #12689, 2.999999999999988898 ) ;
#6568 = ORIENTED_EDGE ( 'NONE', *, *, #5544, .F. ) ;
#6569 = ORIENTED_EDGE ( 'NONE', *, *, #11440, .T. ) ;
#6570 = CARTESIAN_POINT ( 'NONE',  ( 0.000000000000000000, 0.000000000000000000, 3.000000000000000000 ) ) ;
#6571 = FACE_OUTER_BOUND ( 'NONE', #7119, .T. ) ;
#6572 = ADVANCED_FACE ( 'NONE', ( #11556 ), #4498, .T. ) ;
#6573 = EDGE_CURVE ( 'NONE', #1400, #6211, #10535, .T. ) ;
#6574 = VERTEX_POINT ( 'NONE', #6876 ) ;
#6575 =( GEOMETRIC_REPRESENTATION_CONTEXT ( 3 ) GLOBAL_UNCERTAINTY_ASSIGNED_CONTEXT ( ( #9237 ) ) GLOBAL_UNIT_ASSIGNED_CONTEXT ( ( #12640, #6809, #12505 ) ) REPRESENTATION_CONTEXT ( 'NONE', 'WORKASPACE' ) );
#6576 = CARTESIAN_POINT ( 'NONE',  ( -10.40394475573011945, -10.79473832354794460, -5.000000000000000000 ) ) ;
#6577 = COLOUR_RGB ( '',0.8941176470588234615, 0.8941176470588234615, 0.8941176470588234615 ) ;
#6579 = VERTEX_POINT ( 'NONE', #11622 ) ;
#6578 = EDGE_CURVE ( 'NONE', #4401, #12582, #3177, .T. ) ;
#6580 = DIRECTION ( 'NONE',  ( -1.000000000000000000, -0.000000000000000000, -0.000000000000000000 ) ) ;
#6581 = DIRECTION ( 'NONE',  ( 0.9863939238321437486, 0.1643989873053574857, -0.000000000000000000 ) ) ;
#6582 = VECTOR ( 'NONE', #14204, 1000.000000000000114 ) ;
#6583 = AXIS2_PLACEMENT_3D ( 'NONE', #1952, #8781, #783 ) ;
#6584 = ORIENTED_EDGE ( 'NONE', *, *, #9172, .T. ) ;
#6585 = CARTESIAN_POINT ( 'NONE',  ( 0.02436607992775978102, 16.37294372382885044, -18.55949924794875017 ) ) ;
#6586 = CARTESIAN_POINT ( 'NONE',  ( 1.749999999999998002, -27.76164181293049182, -4.147968289691579713 ) ) ;
#6587 = EDGE_LOOP ( 'NONE', ( #13188, #13570, #10897, #14956 ) ) ;
#6588 = EDGE_CURVE ( 'NONE', #2490, #1743, #12800, .T. ) ;
#6589 = ORIENTED_EDGE ( 'NONE', *, *, #11158, .F. ) ;
#6590 = AXIS2_PLACEMENT_3D ( 'NONE', #2001, #1925, #6758 ) ;
#6591 = DIRECTION ( 'NONE',  ( 5.480158469902919838E-17, 1.051478716308701618E-16, 1.000000000000000000 ) ) ;
#6592 = DIRECTION ( 'NONE',  ( 0.8406209333187990573, 0.5416238976136773520, 0.000000000000000000 ) ) ;
#6593 = DIRECTION ( 'NONE',  ( 1.000000000000000000, 0.000000000000000000, 0.000000000000000000 ) ) ;
#6594 = AXIS2_PLACEMENT_3D ( 'NONE', #3030, #10382, #7718 ) ;
#6595 = DIRECTION ( 'NONE',  ( 0.000000000000000000, 1.374038396813314756E-15, -1.000000000000000000 ) ) ;
#6596 = AXIS2_PLACEMENT_3D ( 'NONE', #491, #6267, #8643 ) ;
#6597 = B_SPLINE_CURVE_WITH_KNOTS ( 'NONE', 3,
 ( #1119, #13958, #10722, #10501 ),
 .UNSPECIFIED., .F., .F.,
 ( 4, 4 ),
 ( 0.005123695899043910658, 0.005814329666474868374 ),
 .UNSPECIFIED. ) ;
#6598 = DIRECTION ( 'NONE',  ( 0.000000000000000000, 0.000000000000000000, -1.000000000000000000 ) ) ;
#6599 = FACE_BOUND ( 'NONE', #9133, .T. ) ;
#6600 = LINE ( 'NONE', #7337, #6725 ) ;
#6601 = ORIENTED_EDGE ( 'NONE', *, *, #8347, .T. ) ;
#6602 = DIRECTION ( 'NONE',  ( 0.000000000000000000, 0.000000000000000000, -1.000000000000000000 ) ) ;
#6603 = CARTESIAN_POINT ( 'NONE',  ( 0.006974771092478172958, -9.686319561460797090, -22.53337530003413747 ) ) ;
#6604 = DIRECTION ( 'NONE',  ( -1.000000000000000000, 0.000000000000000000, 0.000000000000000000 ) ) ;
#6605 = ORIENTED_EDGE ( 'NONE', *, *, #5894, .F. ) ;
#6606 = AXIS2_PLACEMENT_3D ( 'NONE', #10513, #14036, #14113 ) ;
#6607 = AXIS2_PLACEMENT_3D ( 'NONE', #12558, #7578, #2033 ) ;
#6608 = CARTESIAN_POINT ( 'NONE',  ( 2.789999999999999147, -11.07980565117273386, -9.999777909380050289 ) ) ;
#6609 = CARTESIAN_POINT ( 'NONE',  ( -0.1085714285714285687, -3.798448662927795372, 0.000000000000000000 ) ) ;
#6610 = ORIENTED_EDGE ( 'NONE', *, *, #11532, .F. ) ;
#6611 = ORIENTED_EDGE ( 'NONE', *, *, #14066, .T. ) ;
#6612 = ADVANCED_FACE ( 'NONE', ( #2333 ), #1107, .T. ) ;
#6613 = DIRECTION ( 'NONE',  ( 0.000000000000000000, 0.000000000000000000, -1.000000000000000000 ) ) ;
#6614 = DIRECTION ( 'NONE',  ( -1.000000000000000000, 0.000000000000000000, 0.000000000000000000 ) ) ;
#6615 = CARTESIAN_POINT ( 'NONE',  ( 2.604434261026088215, -5.253342437939904741, 25.39738473784999684 ) ) ;
#6616 = DIRECTION ( 'NONE',  ( -0.000000000000000000, -0.000000000000000000, -1.000000000000000000 ) ) ;
#6617 = PLANE ( 'NONE',  #13860 ) ;
#6618 = B_SPLINE_CURVE_WITH_KNOTS ( 'NONE', 3,
 ( #12663, #12591, #990, #3231 ),
 .UNSPECIFIED., .F., .F.,
 ( 4, 4 ),
 ( 0.005258214619651984008, 0.005948481662034168192 ),
 .UNSPECIFIED. ) ;
#6619 = DIRECTION ( 'NONE',  ( 0.000000000000000000, 0.000000000000000000, 1.000000000000000000 ) ) ;
#6620 = DIRECTION ( 'NONE',  ( -1.000000000000000000, 0.000000000000000000, 0.000000000000000000 ) ) ;
#6621 = CIRCLE ( 'NONE', #12244, 17.95481323787947758 ) ;
#6622 = ADVANCED_FACE ( 'NONE', ( #12844 ), #7019, .F. ) ;
#6623 = VERTEX_POINT ( 'NONE', #2643 ) ;
#6624 = LINE ( 'NONE', #13762, #3106 ) ;
#6625 = DIRECTION ( 'NONE',  ( 1.000000000000000000, 0.000000000000000000, 0.000000000000000000 ) ) ;
#6626 = VERTEX_POINT ( 'NONE', #10786 ) ;
#6627 = ORIENTED_EDGE ( 'NONE', *, *, #8327, .T. ) ;
#6628 = ORIENTED_EDGE ( 'NONE', *, *, #3464, .F. ) ;
#6629 = ORIENTED_EDGE ( 'NONE', *, *, #10695, .T. ) ;
#6630 = AXIS2_PLACEMENT_3D ( 'NONE', #6385, #12134, #9688 ) ;
#6631 = CARTESIAN_POINT ( 'NONE',  ( 2.715264245299034318, -11.74839219818094982, 9.749517823373967218 ) ) ;
#6632 = CARTESIAN_POINT ( 'NONE',  ( -14.40394475573011945, -13.79473832354794993, 22.00000000000000000 ) ) ;
#6633 = CARTESIAN_POINT ( 'NONE',  ( 0.7592463896980057303, -19.86438386685674473, 19.12676442129336252 ) ) ;
#6634 = EDGE_CURVE ( 'NONE', #3107, #2099, #13156, .T. ) ;
#6635 = VERTEX_POINT ( 'NONE', #6327 ) ;
#6636 = CARTESIAN_POINT ( 'NONE',  ( 2.787319300893938756, -13.26676317347970091, -5.214906618939852301 ) ) ;
#6637 = DIRECTION ( 'NONE',  ( 1.000000000000000000, 0.000000000000000000, 0.000000000000000000 ) ) ;
#6638 = AXIS2_PLACEMENT_3D ( 'NONE', #11517, #6619, #994 ) ;
#6639 = DIRECTION ( 'NONE',  ( 0.000000000000000000, -0.8090169943749444537, -0.5877852522924771339 ) ) ;
#6640 = ADVANCED_FACE ( 'NONE', ( #5117 ), #1555, .F. ) ;
#6641 = CARTESIAN_POINT ( 'NONE',  ( 62.65957446808508280, 26.91300136313512681, 7.000000000000000000 ) ) ;
#6642 = APPLICATION_CONTEXT ( 'automotive_design' ) ;
#6643 = EDGE_LOOP ( 'NONE', ( #6319, #2795, #10227, #9099 ) ) ;
#6644 = DIRECTION ( 'NONE',  ( -0.000000000000000000, -0.000000000000000000, -1.000000000000000000 ) ) ;
#6645 = DIRECTION ( 'NONE',  ( 1.000000000000000000, 0.000000000000000000, 0.000000000000000000 ) ) ;
#6646 = VERTEX_POINT ( 'NONE', #395 ) ;
#6647 = EDGE_LOOP ( 'NONE', ( #8478, #8489, #12927, #11948 ) ) ;
#6648 = CARTESIAN_POINT ( 'NONE',  ( 1.960886852992497653, -24.44424927289185590, 12.96989951879399072 ) ) ;
#6649 = EDGE_CURVE ( 'NONE', #1940, #14933, #14087, .T. ) ;
#6650 = ADVANCED_FACE ( 'NONE', ( #2720 ), #12001, .F. ) ;
#6651 = CYLINDRICAL_SURFACE ( 'NONE', #7743, 28.06981291497571362 ) ;
#6652 = VERTEX_POINT ( 'NONE', #3952 ) ;
#6653 = FACE_OUTER_BOUND ( 'NONE', #7730, .T. ) ;
#6654 = VERTEX_POINT ( 'NONE', #1487 ) ;
#6655 = DIRECTION ( 'NONE',  ( 5.480158469902919838E-17, 1.051478716308701618E-16, 1.000000000000000000 ) ) ;
#6656 = CYLINDRICAL_SURFACE ( 'NONE', #3490, 4.000000000000000000 ) ;
#6657 = VERTEX_POINT ( 'NONE', #4954 ) ;
#6658 = LINE ( 'NONE', #2112, #2151 ) ;
#6659 = DIRECTION ( 'NONE',  ( 0.000000000000000000, 1.000000000000000000, -1.084202172485504187E-16 ) ) ;
#6660 = ORIENTED_EDGE ( 'NONE', *, *, #7614, .F. ) ;
#6661 = EDGE_CURVE ( 'NONE', #10903, #6696, #13723, .T. ) ;
#6662 = ORIENTED_EDGE ( 'NONE', *, *, #9473, .T. ) ;
#6663 = CARTESIAN_POINT ( 'NONE',  ( 2.789999999999999147, 0.000000000000000000, 0.000000000000000000 ) ) ;
#6664 = CARTESIAN_POINT ( 'NONE',  ( 1.749999999999998002, 12.52377138324224148, 25.12109765559658570 ) ) ;
#6665 = EDGE_CURVE ( 'NONE', #13379, #8240, #13194, .T. ) ;
#6666 = CARTESIAN_POINT ( 'NONE',  ( -10.40394475573011945, -10.79473832354794460, -3.000000000000000444 ) ) ;
#6667 = CARTESIAN_POINT ( 'NONE',  ( 1.039999999999996039, 24.89775460606832169, 12.96210679857795256 ) ) ;
#6668 = APPLICATION_PROTOCOL_DEFINITION ( 'draft international standard', 'automotive_design', 1998, #13103 ) ;
#6669 = CARTESIAN_POINT ( 'NONE',  ( 1.039999999999997815, -12.55714665599996316, 12.83329210556827604 ) ) ;
#6670 = CARTESIAN_POINT ( 'NONE',  ( -14.40394475573011945, -10.79473832354794460, 0.7999999999999960476 ) ) ;
#6671 = EDGE_CURVE ( 'NONE', #12582, #13265, #4389, .T. ) ;
#6672 = EDGE_LOOP ( 'NONE', ( #7944, #1735, #9983, #10653 ) ) ;
#6673 = CYLINDRICAL_SURFACE ( 'NONE', #945, 2.524999999999999467 ) ;
#6674 = FACE_OUTER_BOUND ( 'NONE', #1135, .T. ) ;
#6675 = CARTESIAN_POINT ( 'NONE',  ( 2.789999999999999147, -5.229914364928256454, -13.68080036884353845 ) ) ;
#6676 = ORIENTED_EDGE ( 'NONE', *, *, #5389, .F. ) ;
#6677 = CARTESIAN_POINT ( 'NONE',  ( 0.000000000000000000, 13.40591150984226587, 7.739906618939754956 ) ) ;
#6678 = CARTESIAN_POINT ( 'NONE',  ( 2.789999999999999147, 12.52067188844381107, -20.62201879784899461 ) ) ;
#6679 = VERTEX_POINT ( 'NONE', #3636 ) ;
#6680 = EDGE_LOOP ( 'NONE', ( #13494, #14460, #7445, #3173 ) ) ;
#6681 = CYLINDRICAL_SURFACE ( 'NONE', #11702, 13.19999999999999929 ) ;
#6682 = CARTESIAN_POINT ( 'NONE',  ( -9.999999999999998224, 0.000000000000000000, 7.000000000000000000 ) ) ;
#6683 = VERTEX_POINT ( 'NONE', #8323 ) ;
#6684 = CARTESIAN_POINT ( 'NONE',  ( 2.718131847775119514, -5.344160105508880321, 24.78765742476137035 ) ) ;
#6685 = FACE_OUTER_BOUND ( 'NONE', #2765, .T. ) ;
#6686 = CARTESIAN_POINT ( 'NONE',  ( -2.141980652367355020, -6.189445006155633422, -0.8000000000000000444 ) ) ;
#6687 = VECTOR ( 'NONE', #3660, 1000.000000000000000 ) ;
#6688 = CARTESIAN_POINT ( 'NONE',  ( -20.63749999999999574, 0.000000000000000000, -5.400000000000000355 ) ) ;
#6689 = FACE_OUTER_BOUND ( 'NONE', #9399, .T. ) ;
#6690 = ORIENTED_EDGE ( 'NONE', *, *, #13311, .T. ) ;
#6691 = CARTESIAN_POINT ( 'NONE',  ( 0.006974674093433516284, 24.42374957165205629, -2.249040938978583259 ) ) ;
#6692 = B_SPLINE_CURVE_WITH_KNOTS ( 'NONE', 3,
 ( #1501, #13542, #13015, #14189 ),
 .UNSPECIFIED., .F., .F.,
 ( 4, 4 ),
 ( 0.005258139959819257275, 0.005342776758202955750 ),
 .UNSPECIFIED. ) ;
#6693 = CARTESIAN_POINT ( 'NONE',  ( 4.000000000000000888, 4.898587196589413815E-16, 10.00000000000000000 ) ) ;
#6694 = ORIENTED_EDGE ( 'NONE', *, *, #8303, .F. ) ;
#6695 = VECTOR ( 'NONE', #7206, 1000.000000000000000 ) ;
#6696 = VERTEX_POINT ( 'NONE', #9626 ) ;
#6697 = VERTEX_POINT ( 'NONE', #12999 ) ;
#6698 = VERTEX_POINT ( 'NONE', #10854 ) ;
#6699 = DIRECTION ( 'NONE',  ( 0.000000000000000000, 0.000000000000000000, 1.000000000000000000 ) ) ;
#6700 = ADVANCED_FACE ( 'NONE', ( #6246 ), #13442, .T. ) ;
#6701 = FACE_OUTER_BOUND ( 'NONE', #5558, .T. ) ;
#6702 = ORIENTED_EDGE ( 'NONE', *, *, #14364, .F. ) ;
#6703 = CARTESIAN_POINT ( 'NONE',  ( 0.1855654851361731306, 23.63475234378982748, 10.67816411292173306 ) ) ;
#6704 = DIRECTION ( 'NONE',  ( -1.000000000000000000, -0.000000000000000000, -0.000000000000000000 ) ) ;
#6705 = DIRECTION ( 'NONE',  ( 0.000000000000000000, 0.000000000000000000, -1.000000000000000000 ) ) ;
#6706 = EDGE_CURVE ( 'NONE', #2360, #11849, #3635, .T. ) ;
#6707 = B_SPLINE_CURVE_WITH_KNOTS ( 'NONE', 3,
 ( #2758, #14451, #4149, #13515 ),
 .UNSPECIFIED., .F., .F.,
 ( 4, 4 ),
 ( 0.005258120783916788929, 0.005948386350302939385 ),
 .UNSPECIFIED. ) ;
#6708 = ORIENTED_EDGE ( 'NONE', *, *, #5365, .T. ) ;
#6709 = LINE ( 'NONE', #4336, #872 ) ;
#6710 = ADVANCED_FACE ( 'NONE', ( #12154 ), #1178, .T. ) ;
#6711 = DIRECTION ( 'NONE',  ( -1.000000000000000000, 0.000000000000000000, -0.000000000000000000 ) ) ;
#6712 = VERTEX_POINT ( 'NONE', #7172 ) ;
#6713 = VERTEX_POINT ( 'NONE', #8389 ) ;
#6714 = PRESENTATION_STYLE_ASSIGNMENT (( #13718 ) ) ;
#6715 = DIRECTION ( 'NONE',  ( 1.000000000000000000, 0.000000000000000000, 0.000000000000000000 ) ) ;
#6716 = AXIS2_PLACEMENT_3D ( 'NONE', #3672, #8282, #9590 ) ;
#6717 = ORIENTED_EDGE ( 'NONE', *, *, #10701, .T. ) ;
#6718 = CARTESIAN_POINT ( 'NONE',  ( 56.98919079003883326, 3.953582723775848962, 6.000000000000000000 ) ) ;
#6719 = ORIENTED_EDGE ( 'NONE', *, *, #3928, .T. ) ;
#6720 = DIRECTION ( 'NONE',  ( 0.000000000000000000, 0.000000000000000000, -1.000000000000000000 ) ) ;
#6721 = LINE ( 'NONE', #13493, #10852 ) ;
#6722 = ORIENTED_EDGE ( 'NONE', *, *, #3738, .T. ) ;
#6723 = CARTESIAN_POINT ( 'NONE',  ( 2.789999999999999147, -15.04425356660744839, -20.70663861606288236 ) ) ;
#6724 = EDGE_CURVE ( 'NONE', #5016, #10618, #426, .T. ) ;
#6725 = VECTOR ( 'NONE', #3634, 1000.000000000000114 ) ;
#6726 = PLANE ( 'NONE',  #5576 ) ;
#6727 = ORIENTED_EDGE ( 'NONE', *, *, #8757, .T. ) ;
#6728 = ORIENTED_EDGE ( 'NONE', *, *, #146, .F. ) ;
#6729 = CARTESIAN_POINT ( 'NONE',  ( -6.225199705999128148E-14, 2.096282088614769279, 14.05326139264728624 ) ) ;
#6731 = CYLINDRICAL_SURFACE ( 'NONE', #7579, 13.19999999999999929 ) ;
#6730 = AXIS2_PLACEMENT_3D ( 'NONE', #12218, #524, #2995 ) ;
#6732 = AXIS2_PLACEMENT_3D ( 'NONE', #1639, #13157, #11922 ) ;
#6733 = ADVANCED_FACE ( 'NONE', ( #12239 ), #8929, .F. ) ;
#6734 = DIRECTION ( 'NONE',  ( 1.000000000000000000, 0.000000000000000000, 0.000000000000000000 ) ) ;
#6735 = AXIS2_PLACEMENT_3D ( 'NONE', #5327, #8840, #7691 ) ;
#6736 = FACE_OUTER_BOUND ( 'NONE', #9719, .T. ) ;
#6737 = CARTESIAN_POINT ( 'NONE',  ( 2.789999999999999147, -1.991882183130126549, -24.04302995059967429 ) ) ;
#6738 = B_SPLINE_CURVE_WITH_KNOTS ( 'NONE', 3,
 ( #7382, #512, #1609, #14678, #3987, #14453 ),
 .UNSPECIFIED., .F., .F.,
 ( 4, 2, 4 ),
 ( 0.0004963285629697519611, 0.002127826186449857486, 0.003759323809929962686 ),
 .UNSPECIFIED. ) ;
#6739 = CYLINDRICAL_SURFACE ( 'NONE', #8102, 3.799999999999998934 ) ;
#6740 = ADVANCED_FACE ( 'NONE', ( #7867 ), #10016, .T. ) ;
#6741 = ORIENTED_EDGE ( 'NONE', *, *, #6573, .F. ) ;
#6742 = DIRECTION ( 'NONE',  ( 1.445602896647338917E-16, -1.000000000000000000, 0.000000000000000000 ) ) ;
#6743 = DIRECTION ( 'NONE',  ( -0.5416238976136773520, 0.8406209333187989463, 0.000000000000000000 ) ) ;
#6744 = CIRCLE ( 'NONE', #2328, 4.000000000000000888 ) ;
#6745 = DIRECTION ( 'NONE',  ( -1.000000000000000000, -0.000000000000000000, 0.000000000000000000 ) ) ;
#6746 = ADVANCED_FACE ( 'NONE', ( #6557 ), #13939, .T. ) ;
#6747 = AXIS2_PLACEMENT_3D ( 'NONE', #13065, #7251, #14 ) ;
#6748 = EDGE_CURVE ( 'NONE', #2957, #5872, #9776, .T. ) ;
#6749 = ORIENTED_EDGE ( 'NONE', *, *, #340, .F. ) ;
#6750 = DIRECTION ( 'NONE',  ( 0.000000000000000000, 1.000000000000000000, -1.224646799147353207E-16 ) ) ;
#6751 = DIRECTION ( 'NONE',  ( -1.000000000000000000, 0.000000000000000000, -0.000000000000000000 ) ) ;
#6752 = ORIENTED_EDGE ( 'NONE', *, *, #8413, .F. ) ;
#6753 = ORIENTED_EDGE ( 'NONE', *, *, #9193, .F. ) ;
#6754 = DIRECTION ( 'NONE',  ( -1.000000000000000000, -0.000000000000000000, -0.000000000000000000 ) ) ;
#6755 = DIRECTION ( 'NONE',  ( -1.000000000000000000, -0.000000000000000000, -0.000000000000000000 ) ) ;
#6756 = ORIENTED_EDGE ( 'NONE', *, *, #7871, .T. ) ;
#6757 = DIRECTION ( 'NONE',  ( 0.000000000000000000, 0.000000000000000000, 1.000000000000000000 ) ) ;
#6758 = DIRECTION ( 'NONE',  ( 1.000000000000000000, 0.000000000000000000, 0.000000000000000000 ) ) ;
#6759 = CARTESIAN_POINT ( 'NONE',  ( -9.999999999999998224, 0.000000000000000000, 6.000000000000000000 ) ) ;
#6760 = CARTESIAN_POINT ( 'NONE',  ( -2.321707774797442170, -4.824281976789052351, -0.8000000000000000444 ) ) ;
#6761 = AXIS2_PLACEMENT_3D ( 'NONE', #11546, #4490, #12772 ) ;
#6762 = CARTESIAN_POINT ( 'NONE',  ( 0.07181523211953064201, -23.19431517146941246, 10.24584646439529756 ) ) ;
#6763 = DIRECTION ( 'NONE',  ( 0.1643989873053574580, -0.9863939238321436376, 0.000000000000000000 ) ) ;
#6764 = EDGE_CURVE ( 'NONE', #11452, #4926, #8294, .T. ) ;
#6765 = EDGE_CURVE ( 'NONE', #10729, #8622, #7706, .T. ) ;
#6766 = ORIENTED_EDGE ( 'NONE', *, *, #8614, .T. ) ;
#6767 = LINE ( 'NONE', #2006, #8245 ) ;
#6768 = CARTESIAN_POINT ( 'NONE',  ( 67.23404255319148604, 28.93147646537027384, 6.000000000000000000 ) ) ;
#6769 = EDGE_CURVE ( 'NONE', #15033, #3207, #11869, .T. ) ;
#6770 = VERTEX_POINT ( 'NONE', #7787 ) ;
#6771 = AXIS2_PLACEMENT_3D ( 'NONE', #2781, #544, #5257 ) ;
#6772 = ORIENTED_EDGE ( 'NONE', *, *, #4990, .F. ) ;
#6773 = EDGE_LOOP ( 'NONE', ( #1762, #6589, #11999, #9585, #14175, #6942 ) ) ;
#6774 = ORIENTED_EDGE ( 'NONE', *, *, #313, .F. ) ;
#6775 = DIRECTION ( 'NONE',  ( 0.000000000000000000, 0.000000000000000000, 1.000000000000000000 ) ) ;
#6776 = DIRECTION ( 'NONE',  ( 1.000000000000000000, 0.000000000000000000, 0.000000000000000000 ) ) ;
#6777 = EDGE_CURVE ( 'NONE', #8563, #108, #714, .T. ) ;
#6778 = DIRECTION ( 'NONE',  ( 0.9863939238321436376, 0.1643989873053573192, 0.000000000000000000 ) ) ;
#6779 = DIRECTION ( 'NONE',  ( 0.000000000000000000, 0.000000000000000000, 1.000000000000000000 ) ) ;
#6780 = CIRCLE ( 'NONE', #8476, 14.01039946648073986 ) ;
#6781 = ORIENTED_EDGE ( 'NONE', *, *, #14695, .F. ) ;
#6782 = DIRECTION ( 'NONE',  ( 0.000000000000000000, 6.870191984066572599E-15, -1.000000000000000000 ) ) ;
#6783 = CARTESIAN_POINT ( 'NONE',  ( 0.000000000000000000, 6.123233995736766282E-16, -5.000000000000000000 ) ) ;
#6784 = CARTESIAN_POINT ( 'NONE',  ( 83.50748565343083385, 13.38500995229612478, -2.000000000000000888 ) ) ;
#6785 = ORIENTED_EDGE ( 'NONE', *, *, #13114, .F. ) ;
#6786 = CARTESIAN_POINT ( 'NONE',  ( -10.00000000000000000, 0.000000000000000000, 0.000000000000000000 ) ) ;
#6787 = CIRCLE ( 'NONE', #13151, 2.524999999999998579 ) ;
#6788 = DIRECTION ( 'NONE',  ( -0.9148936170212765839, -0.4036950204470272086, 0.000000000000000000 ) ) ;
#6789 = ORIENTED_EDGE ( 'NONE', *, *, #4867, .T. ) ;
#6790 = EDGE_LOOP ( 'NONE', ( #2493, #12046 ) ) ;
#6791 =( GEOMETRIC_REPRESENTATION_CONTEXT ( 3 ) GLOBAL_UNCERTAINTY_ASSIGNED_CONTEXT ( ( #14552 ) ) GLOBAL_UNIT_ASSIGNED_CONTEXT ( ( #10078, #4546, #10307 ) ) REPRESENTATION_CONTEXT ( 'NONE', 'WORKASPACE' ) );
#6792 = AXIS2_PLACEMENT_3D ( 'NONE', #10408, #87, #13004 ) ;
#6793 =( NAMED_UNIT ( * ) PLANE_ANGLE_UNIT ( ) SI_UNIT ( $, .RADIAN. ) );
#6794 = LINE ( 'NONE', #951, #9945 ) ;
#6795 = EDGE_LOOP ( 'NONE', ( #8648, #1706, #12639, #470 ) ) ;
#6796 = AXIS2_PLACEMENT_3D ( 'NONE', #9877, #14509, #12099 ) ;
#6797 = CYLINDRICAL_SURFACE ( 'NONE', #926, 9.999999999999994671 ) ;
#6798 = ADVANCED_FACE ( 'NONE', ( #14784 ), #13620, .F. ) ;
#6799 = CARTESIAN_POINT ( 'NONE',  ( 0.07186811453410689443, 18.89333555428554590, 16.91241718342006450 ) ) ;
#6800 = FACE_OUTER_BOUND ( 'NONE', #10357, .T. ) ;
#6801 = VECTOR ( 'NONE', #3926, 1000.000000000000000 ) ;
#6802 = ORIENTED_EDGE ( 'NONE', *, *, #9963, .T. ) ;
#6803 = AXIS2_PLACEMENT_3D ( 'NONE', #1065, #7984, #12662 ) ;
#6804 = CARTESIAN_POINT ( 'NONE',  ( 2.765633920072235963, -24.63872515616080960, -2.336989772644527008 ) ) ;
#6805 = AXIS2_PLACEMENT_3D ( 'NONE', #1695, #1839, #5237 ) ;
#6806 = ORIENTED_EDGE ( 'NONE', *, *, #2811, .T. ) ;
#6807 = AXIS2_PLACEMENT_3D ( 'NONE', #7025, #13951, #2196 ) ;
#6808 = ORIENTED_EDGE ( 'NONE', *, *, #140, .T. ) ;
#6809 =( NAMED_UNIT ( * ) PLANE_ANGLE_UNIT ( ) SI_UNIT ( $, .RADIAN. ) );
#6810 = CARTESIAN_POINT ( 'NONE',  ( -1.149999999999998135, 0.000000000000000000, 0.000000000000000000 ) ) ;
#6811 = CIRCLE ( 'NONE', #8773, 4.999999999999999112 ) ;
#6812 = CARTESIAN_POINT ( 'NONE',  ( 0.1713913650100259145, 6.016077400811372436E-16, -4.424999999999999822 ) ) ;
#6813 = DIRECTION ( 'NONE',  ( 0.7573544145849105957, -0.6530040510661073716, -2.853163611803960010E-17 ) ) ;
#6814 = AXIS2_PLACEMENT_3D ( 'NONE', #9407, #14261, #4673 ) ;
#6815 = CARTESIAN_POINT ( 'NONE',  ( -5.209999999999999964, 0.000000000000000000, 0.000000000000000000 ) ) ;
#6816 = AXIS2_PLACEMENT_3D ( 'NONE', #1869, #6704, #11384 ) ;
#6817 = CYLINDRICAL_SURFACE ( 'NONE', #11766, 28.06981291497571362 ) ;
#6818 = ORIENTED_EDGE ( 'NONE', *, *, #9986, .F. ) ;
#6819 = CARTESIAN_POINT ( 'NONE',  ( 1.749999999999998002, 12.96210679857822257, -24.89775460606818669 ) ) ;
#6820 = DIRECTION ( 'NONE',  ( -0.000000000000000000, -0.000000000000000000, 1.000000000000000000 ) ) ;
#6821 = CYLINDRICAL_SURFACE ( 'NONE', #5580, 4.000000000000000888 ) ;
#6822 = ORIENTED_EDGE ( 'NONE', *, *, #13303, .F. ) ;
#6823 = EDGE_CURVE ( 'NONE', #2548, #14792, #12474, .T. ) ;
#6824 = LINE ( 'NONE', #3288, #5572 ) ;
#6826 = B_SPLINE_CURVE_WITH_KNOTS ( 'NONE', 3,
 ( #6205, #350, #5067, #2973 ),
 .UNSPECIFIED., .F., .F.,
 ( 4, 4 ),
 ( 0.005258120783916793266, 0.005948386350302923772 ),
 .UNSPECIFIED. ) ;
#6825 = DIRECTION ( 'NONE',  ( 0.000000000000000000, 0.000000000000000000, 1.000000000000000000 ) ) ;
#6827 = VERTEX_POINT ( 'NONE', #2019 ) ;
#6828 = VECTOR ( 'NONE', #4063, 1000.000000000000227 ) ;
#6829 = CIRCLE ( 'NONE', #7082, 4.872650870659752442 ) ;
#6830 = ORIENTED_EDGE ( 'NONE', *, *, #8239, .F. ) ;
#6831 = DIRECTION ( 'NONE',  ( 0.000000000000000000, 0.000000000000000000, 1.000000000000000000 ) ) ;
#6832 = CARTESIAN_POINT ( 'NONE',  ( 72.49759028996471955, 17.18292470770558822, 7.000000000000000000 ) ) ;
#6833 = ORIENTED_EDGE ( 'NONE', *, *, #4957, .T. ) ;
#6834 = CARTESIAN_POINT ( 'NONE',  ( 2.337784062669524321, -16.32199768300081288, 3.429166897524368984 ) ) ;
#6835 = DIRECTION ( 'NONE',  ( 0.000000000000000000, 0.000000000000000000, 1.000000000000000000 ) ) ;
#6836 = CARTESIAN_POINT ( 'NONE',  ( 55.83172393217232354, 8.817765129169439220, -2.000000000000000888 ) ) ;
#6837 = PRODUCT_DEFINITION ( 'UNKNOWN', '', #1311, #8687 ) ;
#6838 = EDGE_CURVE ( 'NONE', #9357, #11164, #9037, .T. ) ;
#6839 = EDGE_CURVE ( 'NONE', #1110, #6106, #4023, .T. ) ;
#6840 = DIRECTION ( 'NONE',  ( 0.000000000000000000, 1.000000000000000000, -1.084202172485504187E-16 ) ) ;
#6841 = CYLINDRICAL_SURFACE ( 'NONE', #4493, 2.524999999999999467 ) ;
#6842 = EDGE_LOOP ( 'NONE', ( #1005, #10153, #3267, #10389, #10841, #3113 ) ) ;
#6843 = CARTESIAN_POINT ( 'NONE',  ( 2.697960337741387438, 15.03709480088671846, 2.583706482362086110 ) ) ;
#6844 = AXIS2_PLACEMENT_3D ( 'NONE', #15075, #9317, #5560 ) ;
#6845 = AXIS2_PLACEMENT_3D ( 'NONE', #5369, #1972, #5436 ) ;
#6846 = CYLINDRICAL_SURFACE ( 'NONE', #1832, 28.06981291497571362 ) ;
#6847 = ORIENTED_EDGE ( 'NONE', *, *, #11904, .T. ) ;
#6848 =( NAMED_UNIT ( * ) SI_UNIT ( $, .STERADIAN. ) SOLID_ANGLE_UNIT ( ) );
#6849 = ORIENTED_EDGE ( 'NONE', *, *, #10644, .F. ) ;
#6850 = ORIENTED_EDGE ( 'NONE', *, *, #5433, .T. ) ;
#6851 = ORIENTED_EDGE ( 'NONE', *, *, #11681, .F. ) ;
#6852 = EDGE_CURVE ( 'NONE', #12499, #10760, #7635, .T. ) ;
#6853 = DIRECTION ( 'NONE',  ( -1.000000000000000000, -0.000000000000000000, -0.000000000000000000 ) ) ;
#6854 = ADVANCED_FACE ( 'NONE', ( #4182 ), #8853, .F. ) ;
#6855 = DIRECTION ( 'NONE',  ( -1.000000000000000000, 0.000000000000000000, 0.000000000000000000 ) ) ;
#6856 = DIRECTION ( 'NONE',  ( -0.000000000000000000, -0.000000000000000000, -1.000000000000000000 ) ) ;
#6857 = TOROIDAL_SURFACE ( 'NONE', #10534, 14.01039946648073986, 8.000000000000000000 ) ;
#6858 = VECTOR ( 'NONE', #1342, 1000.000000000000000 ) ;
#6859 = ADVANCED_FACE ( 'NONE', ( #14556 ), #15184, .T. ) ;
#6860 = CARTESIAN_POINT ( 'NONE',  ( 1.039999999999997593, 0.000000000000000000, 0.000000000000000000 ) ) ;
#6861 = ORIENTED_EDGE ( 'NONE', *, *, #6588, .T. ) ;
#6862 = FACE_OUTER_BOUND ( 'NONE', #9528, .T. ) ;
#6863 = DIRECTION ( 'NONE',  ( 0.000000000000000000, 1.374038396813314756E-15, -1.000000000000000000 ) ) ;
#6864 = EDGE_CURVE ( 'NONE', #5333, #188, #2652, .T. ) ;
#6865 = VECTOR ( 'NONE', #4557, 1000.000000000000000 ) ;
#6866 = FACE_OUTER_BOUND ( 'NONE', #9650, .T. ) ;
#6867 = VERTEX_POINT ( 'NONE', #13040 ) ;
#6868 = CYLINDRICAL_SURFACE ( 'NONE', #11909, 20.00000000000000000 ) ;
#6869 = LINE ( 'NONE', #10477, #107 ) ;
#6870 = VERTEX_POINT ( 'NONE', #11539 ) ;
#6871 = EDGE_LOOP ( 'NONE', ( #7456, #4452, #2495, #7808 ) ) ;
#6872 = DIRECTION ( 'NONE',  ( 0.000000000000000000, 0.000000000000000000, 1.000000000000000000 ) ) ;
#6873 = AXIS2_PLACEMENT_3D ( 'NONE', #1679, #8734, #9746 ) ;
#6874 = ORIENTED_EDGE ( 'NONE', *, *, #2661, .F. ) ;
#6875 = CARTESIAN_POINT ( 'NONE',  ( 0.1713913650100259145, 0.000000000000000000, 0.000000000000000000 ) ) ;
#6876 = CARTESIAN_POINT ( 'NONE',  ( 0.1999999999999985678, -6.997142273814360713, -0.8000000000000000444 ) ) ;
#6877 = CARTESIAN_POINT ( 'NONE',  ( 0.009068833172775131110, 21.10834851580723992, -12.54305517365597922 ) ) ;
#6878 = CARTESIAN_POINT ( 'NONE',  ( 8.000000000000000000, 0.000000000000000000, 0.000000000000000000 ) ) ;
#6879 = VERTEX_POINT ( 'NONE', #14288 ) ;
#6880 = B_SPLINE_CURVE_WITH_KNOTS ( 'NONE', 3,
 ( #8119, #10643, #12645, #2434, #3498, #15122 ),
 .UNSPECIFIED., .F., .F.,
 ( 4, 2, 4 ),
 ( 2.321268216997094965E-07, 0.001878622960950495756, 0.003757013795079291486 ),
 .UNSPECIFIED. ) ;
#6881 = CARTESIAN_POINT ( 'NONE',  ( 60.23740434540291488, 32.40236306526279009, 7.000000000000000000 ) ) ;
#6882 = FACE_OUTER_BOUND ( 'NONE', #9329, .T. ) ;
#6883 = ORIENTED_EDGE ( 'NONE', *, *, #62, .T. ) ;
#6884 = ORIENTED_EDGE ( 'NONE', *, *, #12938, .F. ) ;
#6885 = CARTESIAN_POINT ( 'NONE',  ( 1.039999999999997593, 0.000000000000000000, 0.000000000000000000 ) ) ;
#6886 = CARTESIAN_POINT ( 'NONE',  ( 75.20570977803312473, 12.97982004111159959, 2.999999999999999112 ) ) ;
#6887 = DIRECTION ( 'NONE',  ( 0.000000000000000000, 0.5877852522924805756, -0.8090169943749421222 ) ) ;
#6888 = CARTESIAN_POINT ( 'NONE',  ( 0.000000000000000000, -9.324097380959594616, 22.25075486061734509 ) ) ;
#6889 = CONTEXT_DEPENDENT_SHAPE_REPRESENTATION ( #9110, #1125 ) ;
#6890 = DIRECTION ( 'NONE',  ( 0.000000000000000000, 0.000000000000000000, 1.000000000000000000 ) ) ;
#6891 = EDGE_CURVE ( 'NONE', #10751, #3287, #3153, .T. ) ;
#6892 = FACE_OUTER_BOUND ( 'NONE', #14761, .T. ) ;
#6893 = ORIENTED_EDGE ( 'NONE', *, *, #10084, .F. ) ;
#6894 = CARTESIAN_POINT ( 'NONE',  ( 86.00000000000000000, 7.347880794884117764E-16, 5.500000000000000000 ) ) ;
#6895 = DIRECTION ( 'NONE',  ( -1.000000000000000000, -0.000000000000000000, -0.000000000000000000 ) ) ;
#6896 = CARTESIAN_POINT ( 'NONE',  ( 2.789999999999999147, 11.07980565117280314, 9.999777909379972129 ) ) ;
#6897 = LINE ( 'NONE', #11575, #1395 ) ;
#6898 = ORIENTED_EDGE ( 'NONE', *, *, #9712, .F. ) ;
#6899 = EDGE_CURVE ( 'NONE', #9813, #5482, #11815, .T. ) ;
#6900 = DIRECTION ( 'NONE',  ( 0.000000000000000000, 1.776356839400252831E-15, -1.000000000000000000 ) ) ;
#6901 = CARTESIAN_POINT ( 'NONE',  ( 2.765633920072235519, 18.55949924794892780, 16.37294372382865504 ) ) ;
#6902 = ORIENTED_EDGE ( 'NONE', *, *, #8026, .F. ) ;
#6903 = VERTEX_POINT ( 'NONE', #5984 ) ;
#6904 = CARTESIAN_POINT ( 'NONE',  ( 1.039999999999997593, 4.835383649608715473, -17.29145405592683815 ) ) ;
#6905 = DIRECTION ( 'NONE',  ( 0.000000000000000000, 0.000000000000000000, 1.000000000000000000 ) ) ;
#6906 = EDGE_CURVE ( 'NONE', #6954, #5429, #12612, .T. ) ;
#6907 = ORIENTED_EDGE ( 'NONE', *, *, #14063, .T. ) ;
#6908 = CARTESIAN_POINT ( 'NONE',  ( 2.236220346785029456, -16.55730827443882447, 3.624349476775136303 ) ) ;
#6909 = DIRECTION ( 'NONE',  ( -1.000000000000000000, -0.000000000000000000, -0.000000000000000000 ) ) ;
#6910 = B_SPLINE_CURVE_WITH_KNOTS ( 'NONE', 3,
 ( #8965, #11347, #12576, #11416 ),
 .UNSPECIFIED., .F., .F.,
 ( 4, 4 ),
 ( 0.0002742066915197750193, 0.0006916721208754025157 ),
 .UNSPECIFIED. ) ;
#6911 = CARTESIAN_POINT ( 'NONE',  ( 1.000000000000000000, -5.408326913195983465, 0.000000000000000000 ) ) ;
#6912 = EDGE_CURVE ( 'NONE', #11615, #6129, #7143, .T. ) ;
#6913 = CARTESIAN_POINT ( 'NONE',  ( 75.20570977803312473, 12.97982004111159959, 2.999999999999999112 ) ) ;
#6914 = PLANE ( 'NONE',  #6978 ) ;
#6915 = VECTOR ( 'NONE', #6476, 1000.000000000000114 ) ;
#6916 = ORIENTED_EDGE ( 'NONE', *, *, #914, .T. ) ;
#6917 = DIRECTION ( 'NONE',  ( 5.480158469902919838E-17, 1.051478716308701618E-16, 1.000000000000000000 ) ) ;
#6918 = CARTESIAN_POINT ( 'NONE',  ( 0.000000000000000000, 8.624777288397805108, 11.04103753892274575 ) ) ;
#6919 = ORIENTED_EDGE ( 'NONE', *, *, #5625, .F. ) ;
#6920 = ADVANCED_FACE ( 'NONE', ( #8288 ), #1293, .T. ) ;
#6921 = EDGE_CURVE ( 'NONE', #12007, #6623, #173, .T. ) ;
#6922 = ORIENTED_EDGE ( 'NONE', *, *, #10233, .F. ) ;
#6923 = ORIENTED_EDGE ( 'NONE', *, *, #7707, .F. ) ;
#6924 = ORIENTED_EDGE ( 'NONE', *, *, #13746, .F. ) ;
#6925 = DIRECTION ( 'NONE',  ( 0.000000000000000000, 0.000000000000000000, -1.000000000000000000 ) ) ;
#6926 = DIRECTION ( 'NONE',  ( 0.9728364810787193395, 0.2314933715733012709, -0.000000000000000000 ) ) ;
#6927 = CIRCLE ( 'NONE', #281, 3.799999999999999378 ) ;
#6928 = CARTESIAN_POINT ( 'NONE',  ( 0.2076372544708503520, -10.30022894898797858, -12.04200105039481095 ) ) ;
#6929 = CARTESIAN_POINT ( 'NONE',  ( -4.000000000000000888, 0.000000000000000000, 10.00000000000000000 ) ) ;
#6930 = DIRECTION ( 'NONE',  ( 0.5416238976136762417, -0.8406209333187997235, -0.000000000000000000 ) ) ;
#6931 = ORIENTED_EDGE ( 'NONE', *, *, #3417, .T. ) ;
#6932 = CARTESIAN_POINT ( 'NONE',  ( 2.790000000000000480, 9.514945144208736494, 22.37986894186676423 ) ) ;
#6933 = ADVANCED_FACE ( 'NONE', ( #10670 ), #10386, .T. ) ;
#6934 = VECTOR ( 'NONE', #13475, 1000.000000000000000 ) ;
#6935 = AXIS2_PLACEMENT_3D ( 'NONE', #14576, #4044, #12261 ) ;
#6936 = CARTESIAN_POINT ( 'NONE',  ( 0.7686372430964468760, 17.00993931356758537, -4.022333916463615822 ) ) ;
#6937 = EDGE_CURVE ( 'NONE', #5435, #11802, #3750, .T. ) ;
#6938 = EDGE_CURVE ( 'NONE', #15169, #2185, #4876, .T. ) ;
#6939 = ORIENTED_EDGE ( 'NONE', *, *, #915, .F. ) ;
#6940 = PLANE ( 'NONE',  #7509 ) ;
#6941 = DIRECTION ( 'NONE',  ( 1.000000000000000000, 0.000000000000000000, 0.000000000000000000 ) ) ;
#6942 = ORIENTED_EDGE ( 'NONE', *, *, #15112, .F. ) ;
#6943 = ORIENTED_EDGE ( 'NONE', *, *, #3509, .T. ) ;
#6944 = VECTOR ( 'NONE', #10792, 1000.000000000000114 ) ;
#6945 = DIRECTION ( 'NONE',  ( 5.782411586589355667E-16, 1.000000000000000000, 0.000000000000000000 ) ) ;
#6946 = VERTEX_POINT ( 'NONE', #12691 ) ;
#6947 = CARTESIAN_POINT ( 'NONE',  ( 1.039999999999996705, 19.67366047555530173, 20.02152543075352398 ) ) ;
#6948 = DIRECTION ( 'NONE',  ( 0.000000000000000000, 0.000000000000000000, 1.000000000000000000 ) ) ;
#6949 = CARTESIAN_POINT ( 'NONE',  ( 2.789999999999999147, 18.28042085475278355, 15.74360496233388140 ) ) ;
#6950 = CARTESIAN_POINT ( 'NONE',  ( -14.40394475573012301, -16.79473832354794993, 13.99999999999999645 ) ) ;
#6951 = ORIENTED_EDGE ( 'NONE', *, *, #12420, .F. ) ;
#6952 = CARTESIAN_POINT ( 'NONE',  ( -16.96657417111497068, -13.60061260430328467, -3.794707603699265519E-15 ) ) ;
#6953 = CARTESIAN_POINT ( 'NONE',  ( 2.765633920072235519, -18.55949924794880346, -16.37294372382878649 ) ) ;
#6954 = VERTEX_POINT ( 'NONE', #10752 ) ;
#6955 = VERTEX_POINT ( 'NONE', #15087 ) ;
#6956 = CARTESIAN_POINT ( 'NONE',  ( 1.749999999999998002, 24.89775460606851354, -12.96210679857759729 ) ) ;
#6957 = DIRECTION ( 'NONE',  ( -1.000000000000000000, -0.000000000000000000, 0.000000000000000000 ) ) ;
#6958 = EDGE_CURVE ( 'NONE', #368, #1565, #10009, .T. ) ;
#6959 = B_SPLINE_CURVE_WITH_KNOTS ( 'NONE', 3,
 ( #8343, #4600, #8051, #13019 ),
 .UNSPECIFIED., .F., .F.,
 ( 4, 4 ),
 ( 0.005258105385878691744, 0.005948373736081389272 ),
 .UNSPECIFIED. ) ;
#6960 = LINE ( 'NONE', #5895, #9020 ) ;
#6961 = CARTESIAN_POINT ( 'NONE',  ( 0.000000000000000000, -20.62201879784923264, 12.52067188844344336 ) ) ;
#6962 = CARTESIAN_POINT ( 'NONE',  ( 50.00050000000000239, 0.000000000000000000, 4.000000000000000000 ) ) ;
#6963 = CARTESIAN_POINT ( 'NONE',  ( 2.765633920072239071, -12.59161484032927092, 21.30679549418627161 ) ) ;
#6964 = ORIENTED_EDGE ( 'NONE', *, *, #11239, .T. ) ;
#6965 = CARTESIAN_POINT ( 'NONE',  ( 2.789999999999999147, -20.62201879784921843, 12.52067188844344336 ) ) ;
#6966 = CARTESIAN_POINT ( 'NONE',  ( 0.000000000000000000, 0.000000000000000000, 1.395000000000000462 ) ) ;
#6967 = CARTESIAN_POINT ( 'NONE',  ( 1.149999999999998135, 0.000000000000000000, 0.000000000000000000 ) ) ;
#6968 = CARTESIAN_POINT ( 'NONE',  ( 1.250000000000001110, 0.000000000000000000, -5.899999999999999467 ) ) ;
#6969 = VERTEX_POINT ( 'NONE', #9437 ) ;
#6970 = EDGE_CURVE ( 'NONE', #11124, #5767, #3391, .T. ) ;
#6971 = CARTESIAN_POINT ( 'NONE',  ( 0.02531912748606228100, -13.68080036884352246, 5.229914364928304416 ) ) ;
#6972 = CARTESIAN_POINT ( 'NONE',  ( 1.885839510111769313, -17.01651022436359995, -4.928563447326470559 ) ) ;
#6973 = CIRCLE ( 'NONE', #7710, 2.524999999999994582 ) ;
#6974 = EDGE_LOOP ( 'NONE', ( #12589, #6003, #13740, #4168 ) ) ;
#6975 = AXIS2_PLACEMENT_3D ( 'NONE', #13070, #11924, #1412 ) ;
#6976 = DIRECTION ( 'NONE',  ( -1.000000000000000000, -0.000000000000000000, 0.000000000000000000 ) ) ;
#6977 = DIRECTION ( 'NONE',  ( 0.000000000000000000, 0.000000000000000000, 1.000000000000000000 ) ) ;
#6978 = AXIS2_PLACEMENT_3D ( 'NONE', #5765, #1225, #7064 ) ;
#6979 = CARTESIAN_POINT ( 'NONE',  ( -9.403944755730117677, -16.79473832354794993, 16.99999999999999645 ) ) ;
#6980 = DIRECTION ( 'NONE',  ( -1.000000000000000000, 0.000000000000000000, 0.000000000000000000 ) ) ;
#6981 = DIRECTION ( 'NONE',  ( -1.000000000000000000, 0.000000000000000000, 0.000000000000000000 ) ) ;
#6982 = CARTESIAN_POINT ( 'NONE',  ( 91.12964445316927709, 15.08873975234342701, 4.000000000000000000 ) ) ;
#6983 = CARTESIAN_POINT ( 'NONE',  ( 2.765633920072237295, 12.59161484032912171, 21.30679549418635688 ) ) ;
#6984 = AXIS2_PLACEMENT_3D ( 'NONE', #3762, #138, #9767 ) ;
#6985 = EDGE_CURVE ( 'NONE', #10552, #7184, #10412, .T. ) ;
#6986 = ORIENTED_EDGE ( 'NONE', *, *, #8379, .T. ) ;
#6987 = CYLINDRICAL_SURFACE ( 'NONE', #10222, 2.999999999999988898 ) ;
#6988 = CIRCLE ( 'NONE', #6491, 17.95481323787947758 ) ;
#6989 = AXIS2_PLACEMENT_3D ( 'NONE', #13991, #3457, #11302 ) ;
#6990 = LINE ( 'NONE', #3523, #12862 ) ;
#6991 = ADVANCED_FACE ( 'NONE', ( #7214 ), #1368, .F. ) ;
#6992 = ORIENTED_EDGE ( 'NONE', *, *, #12540, .T. ) ;
#6993 = EDGE_LOOP ( 'NONE', ( #8617, #6446, #10269, #12887, #1491, #12622, #8690, #2687 ) ) ;
#6994 = ORIENTED_EDGE ( 'NONE', *, *, #6391, .T. ) ;
#6995 = ORIENTED_EDGE ( 'NONE', *, *, #4425, .F. ) ;
#6996 = DIRECTION ( 'NONE',  ( -1.000000000000000000, -0.000000000000000000, -0.000000000000000000 ) ) ;
#6997 = CIRCLE ( 'NONE', #10429, 4.999999999999999112 ) ;
#6998 = CARTESIAN_POINT ( 'NONE',  ( 85.79342132543153809, 17.83186255874426962, -2.000000000000000888 ) ) ;
#6999 = VECTOR ( 'NONE', #12464, 1000.000000000000000 ) ;
#7000 = CARTESIAN_POINT ( 'NONE',  ( -1.249999999999997558, 0.000000000000000000, 0.000000000000000000 ) ) ;
#7001 = FACE_OUTER_BOUND ( 'NONE', #3310, .T. ) ;
#7002 = CARTESIAN_POINT ( 'NONE',  ( 0.09203966225861190398, -2.583706482361930235, -15.03709480088674688 ) ) ;
#7003 = EDGE_LOOP ( 'NONE', ( #4799, #7906, #6830, #10302 ) ) ;
#7004 = DIRECTION ( 'NONE',  ( -0.000000000000000000, -0.000000000000000000, 1.000000000000000000 ) ) ;
#7005 = AXIS2_PLACEMENT_3D ( 'NONE', #13856, #5578, #873 ) ;
#7006 = AXIS2_PLACEMENT_3D ( 'NONE', #5703, #6853, #4475 ) ;
#7007 = EDGE_CURVE ( 'NONE', #9849, #761, #4927, .T. ) ;
#7008 = VERTEX_POINT ( 'NONE', #4414 ) ;
#7009 = LINE ( 'NONE', #4421, #10476 ) ;
#7010 = CARTESIAN_POINT ( 'NONE',  ( 75.20570977803312473, 12.97982004111159959, -2.000000000000000888 ) ) ;
#7011 = B_SPLINE_CURVE_WITH_KNOTS ( 'NONE', 3,
 ( #8241, #11776, #5945, #10629 ),
 .UNSPECIFIED., .F., .F.,
 ( 4, 4 ),
 ( 0.005123713096549380695, 0.005814346476695810180 ),
 .UNSPECIFIED. ) ;
#7012 = ORIENTED_EDGE ( 'NONE', *, *, #4879, .F. ) ;
#7013 = EDGE_LOOP ( 'NONE', ( #8876, #14198, #9917, #15186, #10510, #11036, #1553, #10137, #11775, #4848, #4002, #10040, #4986, #369, #3815, #195, #8844, #5411, #4319, #9466, #13353, #213, #9325, #6849, #4569, #3411, #15047 ) ) ;
#7014 = DIRECTION ( 'NONE',  ( 0.000000000000000000, 0.000000000000000000, 1.000000000000000000 ) ) ;
#7015 = EDGE_CURVE ( 'NONE', #5666, #12669, #7567, .T. ) ;
#7016 = EDGE_CURVE ( 'NONE', #4354, #4613, #937, .T. ) ;
#7017 = ORIENTED_EDGE ( 'NONE', *, *, #6649, .F. ) ;
#7018 = CARTESIAN_POINT ( 'NONE',  ( 2.740003281797976253, 13.99876742897266446, -5.264737421541377138 ) ) ;
#7019 = PLANE ( 'NONE',  #2932 ) ;
#7020 = DIRECTION ( 'NONE',  ( 1.000000000000000000, 0.000000000000000000, 0.000000000000000000 ) ) ;
#7021 = AXIS2_PLACEMENT_3D ( 'NONE', #10973, #4064, #9666 ) ;
#7022 = FACE_OUTER_BOUND ( 'NONE', #10230, .T. ) ;
#7023 = ORIENTED_EDGE ( 'NONE', *, *, #14307, .T. ) ;
#7024 = AXIS2_PLACEMENT_3D ( 'NONE', #6677, #4225, #5533 ) ;
#7025 = CARTESIAN_POINT ( 'NONE',  ( 0.9999999999999997780, -6.008326913195983998, -0.8000000000000000444 ) ) ;
#7026 = DIRECTION ( 'NONE',  ( 0.000000000000000000, 0.000000000000000000, 1.000000000000000000 ) ) ;
#7027 = MECHANICAL_DESIGN_GEOMETRIC_PRESENTATION_REPRESENTATION (  '', ( #11447 ), #6791 ) ;
#7028 = VERTEX_POINT ( 'NONE', #7527 ) ;
#7029 = ORIENTED_EDGE ( 'NONE', *, *, #4466, .T. ) ;
#7030 = EDGE_CURVE ( 'NONE', #12603, #2895, #8819, .T. ) ;
#7031 = CARTESIAN_POINT ( 'NONE',  ( 2.765633920072235963, 21.30679549418649543, -12.59161484032888723 ) ) ;
#7032 = LINE ( 'NONE', #3570, #9048 ) ;
#7033 = EDGE_CURVE ( 'NONE', #4224, #7818, #13453, .T. ) ;
#7034 = AXIS2_PLACEMENT_3D ( 'NONE', #11502, #7904, #5748 ) ;
#7035 = AXIS2_PLACEMENT_3D ( 'NONE', #144, #1391, #3619 ) ;
#7036 = DIRECTION ( 'NONE',  ( -1.000000000000000000, -0.000000000000000000, -0.000000000000000000 ) ) ;
#7037 = DIRECTION ( 'NONE',  ( 1.000000000000000000, 0.000000000000000000, 0.000000000000000000 ) ) ;
#7038 = CONTEXT_DEPENDENT_SHAPE_REPRESENTATION ( #3316, #15123 ) ;
#7039 = DIRECTION ( 'NONE',  ( -1.000000000000000000, -0.000000000000000000, -0.000000000000000000 ) ) ;
#7040 = ADVANCED_FACE ( 'NONE', ( #8513 ), #6141, .F. ) ;
#7041 = AXIS2_PLACEMENT_3D ( 'NONE', #135, #12825, #5929 ) ;
#7042 = DIRECTION ( 'NONE',  ( 0.000000000000000000, 0.000000000000000000, 1.000000000000000000 ) ) ;
#7043 = VECTOR ( 'NONE', #13877, 1000.000000000000000 ) ;
#7044 = ORIENTED_EDGE ( 'NONE', *, *, #8116, .F. ) ;
#7045 = DIRECTION ( 'NONE',  ( -0.000000000000000000, -0.000000000000000000, -1.000000000000000000 ) ) ;
#7046 = FACE_OUTER_BOUND ( 'NONE', #13818, .T. ) ;
#7047 = CARTESIAN_POINT ( 'NONE',  ( 2.789999999999999147, 12.98979500319701508, -5.249430348645618416 ) ) ;
#7048 = CYLINDRICAL_SURFACE ( 'NONE', #3848, 28.06981291497571362 ) ;
#7049 = EDGE_CURVE ( 'NONE', #10081, #9211, #12115, .T. ) ;
#7050 = CIRCLE ( 'NONE', #13678, 2.524999999999999023 ) ;
#7051 = ORIENTED_EDGE ( 'NONE', *, *, #2784, .F. ) ;
#7052 = VERTEX_POINT ( 'NONE', #2911 ) ;
#7053 = CARTESIAN_POINT ( 'NONE',  ( 2.010451917295053459, -16.73367785739753444, -5.008579424861741458 ) ) ;
#7054 = ORIENTED_EDGE ( 'NONE', *, *, #6912, .T. ) ;
#7055 = CIRCLE ( 'NONE', #6814, 3.799999999999999378 ) ;
#7056 = CARTESIAN_POINT ( 'NONE',  ( 1.885839528871395609, 12.77651625388916301, -12.27244837507599762 ) ) ;
#7057 = CARTESIAN_POINT ( 'NONE',  ( 75.68384697807671557, 11.35494834827056110, 6.000000000000000000 ) ) ;
#7058 = CIRCLE ( 'NONE', #196, 3.000000000000000888 ) ;
#7059 = AXIS2_PLACEMENT_3D ( 'NONE', #14873, #3120, #3035 ) ;
#7060 = CARTESIAN_POINT ( 'NONE',  ( 1.394999999999999574, -12.55714665599978019, -12.83329210556845013 ) ) ;
#7061 = FACE_OUTER_BOUND ( 'NONE', #2031, .T. ) ;
#7062 = CARTESIAN_POINT ( 'NONE',  ( 2.765633920072234631, 5.391175441198615914, 24.15498966839965078 ) ) ;
#7063 = CARTESIAN_POINT ( 'NONE',  ( -20.63749999999999929, 0.000000000000000000, 0.000000000000000000 ) ) ;
#7064 = DIRECTION ( 'NONE',  ( 0.9728364810787194505, 0.2314933715733012709, 0.000000000000000000 ) ) ;
#7065 = EDGE_LOOP ( 'NONE', ( #11486, #1029, #11322, #2010 ) ) ;
#7066 = CARTESIAN_POINT ( 'NONE',  ( 2.789999999999999147, -22.25075486061744812, 9.324097380959361914 ) ) ;
#7067 = AXIS2_PLACEMENT_3D ( 'NONE', #10545, #11979, #10688 ) ;
#7068 = DIRECTION ( 'NONE',  ( 0.9148936170212765839, 0.4036950204470272086, -0.000000000000000000 ) ) ;
#7069 = AXIS2_PLACEMENT_3D ( 'NONE', #6054, #1218, #9427 ) ;
#7070 = ORIENTED_EDGE ( 'NONE', *, *, #11956, .T. ) ;
#7071 = AXIS2_PLACEMENT_3D ( 'NONE', #13388, #2866, #7562 ) ;
#7072 = VERTEX_POINT ( 'NONE', #13276 ) ;
#7073 = EDGE_LOOP ( 'NONE', ( #14548, #607, #13745, #4950 ) ) ;
#7074 = ORIENTED_EDGE ( 'NONE', *, *, #11618, .T. ) ;
#7075 = B_SPLINE_CURVE_WITH_KNOTS ( 'NONE', 3,
 ( #14934, #11377, #5559, #2168, #14851, #13771 ),
 .UNSPECIFIED., .F., .F.,
 ( 4, 2, 4 ),
 ( 4.462636731831954487E-07, 0.001879885066974966781, 0.003759323870276750149 ),
 .UNSPECIFIED. ) ;
#7076 = CARTESIAN_POINT ( 'NONE',  ( 0.2291144030788790364, -15.06658931286050951, 5.279841123860816055 ) ) ;
#7077 = CARTESIAN_POINT ( 'NONE',  ( 0.9041604898882319441, -4.928563447326170355, -17.01651022436368876 ) ) ;
#7078 = AXIS2_PLACEMENT_3D ( 'NONE', #13446, #14465, #1765 ) ;
#7079 = DIRECTION ( 'NONE',  ( -0.000000000000000000, -0.000000000000000000, -1.000000000000000000 ) ) ;
#7080 = DIRECTION ( 'NONE',  ( 0.000000000000000000, -1.000000000000000000, 0.000000000000000000 ) ) ;
#7081 = DIRECTION ( 'NONE',  ( 0.4036950204470249881, -0.9148936170212775831, 0.000000000000000000 ) ) ;
#7082 = AXIS2_PLACEMENT_3D ( 'NONE', #3649, #7186, #7114 ) ;
#7083 = TOROIDAL_SURFACE ( 'NONE', #443, 5.000000000000000000, 0.5999999999999999778 ) ;
#7084 = EDGE_LOOP ( 'NONE', ( #10105, #6345, #9863, #4393 ) ) ;
#7085 = LINE ( 'NONE', #4083, #9006 ) ;
#7086 = AXIS2_PLACEMENT_3D ( 'NONE', #2284, #1349, #4825 ) ;
#7087 = AXIS2_PLACEMENT_3D ( 'NONE', #8715, #13408, #2662 ) ;
#7088 = ORIENTED_EDGE ( 'NONE', *, *, #942, .T. ) ;
#7089 = AXIS2_PLACEMENT_3D ( 'NONE', #7964, #96, #6890 ) ;
#7090 = DIRECTION ( 'NONE',  ( -1.000000000000000000, -0.000000000000000000, -0.000000000000000000 ) ) ;
#7091 = CYLINDRICAL_SURFACE ( 'NONE', #10190, 13.19999999999999929 ) ;
#7092 = B_SPLINE_CURVE_WITH_KNOTS ( 'NONE', 3,
 ( #9098, #3188, #7870, #633, #4185, #8855 ),
 .UNSPECIFIED., .F., .F.,
 ( 4, 2, 4 ),
 ( 4.462636732176736601E-07, 0.001879885066974997356, 0.003759323870276777037 ),
 .UNSPECIFIED. ) ;
#7093 = ORIENTED_EDGE ( 'NONE', *, *, #12295, .T. ) ;
#7094 = ORIENTED_EDGE ( 'NONE', *, *, #9384, .F. ) ;
#7095 = ADVANCED_FACE ( 'NONE', ( #14524 ), #12041, .T. ) ;
#7096 = CARTESIAN_POINT ( 'NONE',  ( 2.783025228907520798, -22.53337530003396338, -9.686319561461189664 ) ) ;
#7097 = VERTEX_POINT ( 'NONE', #7669 ) ;
#7098 = DIRECTION ( 'NONE',  ( -1.000000000000000000, -0.000000000000000000, 0.000000000000000000 ) ) ;
#7099 = EDGE_CURVE ( 'NONE', #1547, #12081, #9681, .T. ) ;
#7100 = DIRECTION ( 'NONE',  ( 1.000000000000000000, -0.000000000000000000, 0.000000000000000000 ) ) ;
#7101 = B_SPLINE_CURVE_WITH_KNOTS ( 'NONE', 3,
 ( #2205, #4212, #8882, #4361 ),
 .UNSPECIFIED., .F., .F.,
 ( 4, 4 ),
 ( 2.034713381942769504E-07, 0.0006887909409525124101 ),
 .UNSPECIFIED. ) ;
#7102 = VECTOR ( 'NONE', #11368, 1000.000000000000000 ) ;
#7103 = CARTESIAN_POINT ( 'NONE',  ( 0.5321745087963408727, 11.58891744060107065, 24.44564404695848836 ) ) ;
#7104 = CARTESIAN_POINT ( 'NONE',  ( 2.135044773435426091, -16.44225436089929815, 5.086950209440439075 ) ) ;
#7105 = VERTEX_POINT ( 'NONE', #3829 ) ;
#7106 = FACE_OUTER_BOUND ( 'NONE', #8073, .T. ) ;
#7107 = DIRECTION ( 'NONE',  ( -0.000000000000000000, -0.000000000000000000, 1.000000000000000000 ) ) ;
#7108 = ORIENTED_EDGE ( 'NONE', *, *, #13691, .T. ) ;
#7109 = ADVANCED_FACE ( 'NONE', ( #2982 ), #10823, .F. ) ;
#7110 = ADVANCED_FACE ( 'NONE', ( #1605 ), #12710, .T. ) ;
#7111 = ORIENTED_EDGE ( 'NONE', *, *, #11225, .F. ) ;
#7112 = LINE ( 'NONE', #5956, #13189 ) ;
#7113 = CIRCLE ( 'NONE', #1348, 14.01039946648074341 ) ;
#7114 = DIRECTION ( 'NONE',  ( 1.000000000000000000, 0.000000000000000000, 0.000000000000000000 ) ) ;
#7115 = DIRECTION ( 'NONE',  ( -1.000000000000000000, -0.000000000000000000, -0.000000000000000000 ) ) ;
#7116 = CYLINDRICAL_SURFACE ( 'NONE', #4061, 3.000000000000002665 ) ;
#7117 = DIRECTION ( 'NONE',  ( 0.000000000000000000, -0.9510565162951544194, 0.3090169943749446757 ) ) ;
#7118 = CARTESIAN_POINT ( 'NONE',  ( 2.764680872513688659, 2.311161484776556030, 14.46287784598618309 ) ) ;
#7119 = EDGE_LOOP ( 'NONE', ( #12491, #14376, #12585, #4544, #13382, #1740 ) ) ;
#7120 = CARTESIAN_POINT ( 'NONE',  ( 0.000000000000000000, 0.000000000000000000, 0.000000000000000000 ) ) ;
#7121 = DIRECTION ( 'NONE',  ( 0.000000000000000000, 0.000000000000000000, 1.000000000000000000 ) ) ;
#7122 = CARTESIAN_POINT ( 'NONE',  ( 1.039999999999997149, -27.68468304288261805, 4.633866840648821039 ) ) ;
#7123 = AXIS2_PLACEMENT_3D ( 'NONE', #7358, #7503, #4039 ) ;
#7124 = FACE_OUTER_BOUND ( 'NONE', #14960, .T. ) ;
#7125 = EDGE_CURVE ( 'NONE', #1757, #6626, #10021, .T. ) ;
#7126 = VERTEX_POINT ( 'NONE', #13349 ) ;
#7127 = VERTEX_POINT ( 'NONE', #2829 ) ;
#7128 = EDGE_CURVE ( 'NONE', #14060, #4311, #10757, .T. ) ;
#7129 =( NAMED_UNIT ( * ) SI_UNIT ( $, .STERADIAN. ) SOLID_ANGLE_UNIT ( ) );
#7130 = EDGE_LOOP ( 'NONE', ( #4402, #12637, #13898, #13580 ) ) ;
#7131 = B_SPLINE_CURVE_WITH_KNOTS ( 'NONE', 3,
 ( #2309, #1164, #11170, #9944 ),
 .UNSPECIFIED., .F., .F.,
 ( 4, 4 ),
 ( 1.988537749986029444E-07, 0.0006916721208753980705 ),
 .UNSPECIFIED. ) ;
#7132 = DIRECTION ( 'NONE',  ( 0.000000000000000000, 0.000000000000000000, 1.000000000000000000 ) ) ;
#7133 = CARTESIAN_POINT ( 'NONE',  ( 2.790000000000000924, 4.898587196589412829E-16, -4.000000000000000000 ) ) ;
#7134 = CARTESIAN_POINT ( 'NONE',  ( 1.039999999999998925, -17.29145405592692342, 4.835383649608409939 ) ) ;
#7135 = CARTESIAN_POINT ( 'NONE',  ( 2.021362784118871936, 11.98841295390615613, -12.71987259277422844 ) ) ;
#7136 = CARTESIAN_POINT ( 'NONE',  ( 80.00000000000000000, 3.469446951953614189E-15, 5.750000000000001776 ) ) ;
#7137 = CARTESIAN_POINT ( 'NONE',  ( 98.33955663538051795, 3.898681236723621879, 7.000000000000000000 ) ) ;
#7138 = EDGE_CURVE ( 'NONE', #14234, #12512, #6367, .T. ) ;
#7139 = ORIENTED_EDGE ( 'NONE', *, *, #5405, .T. ) ;
#7140 = DIRECTION ( 'NONE',  ( 0.000000000000000000, 0.000000000000000000, -1.000000000000000000 ) ) ;
#7141 = CARTESIAN_POINT ( 'NONE',  ( 0.000000000000000000, 22.25075486061751207, -9.324097380959241121 ) ) ;
#7142 = ORIENTED_EDGE ( 'NONE', *, *, #14651, .T. ) ;
#7143 = LINE ( 'NONE', #3251, #5124 ) ;
#7144 = CARTESIAN_POINT ( 'NONE',  ( 98.48580539929344013, 0.9022481406819604643, -2.000000000000000888 ) ) ;
#7145 = PRODUCT_DEFINITION_SHAPE ( 'NONE', 'NONE',  #15244 ) ;
#7146 = CARTESIAN_POINT ( 'NONE',  ( 70.16198417812034904, 9.730076655429538590, 6.000000000000000000 ) ) ;
#7147 = VERTEX_POINT ( 'NONE', #9892 ) ;
#7148 = SURFACE_STYLE_USAGE ( .BOTH. , #2465 ) ;
#7149 = VERTEX_POINT ( 'NONE', #11118 ) ;
#7150 = ORIENTED_EDGE ( 'NONE', *, *, #11812, .F. ) ;
#7151 = VERTEX_POINT ( 'NONE', #14592 ) ;
#7152 = CARTESIAN_POINT ( 'NONE',  ( 0.3493891680732006955, -15.53033051714692547, 5.240368680323494566 ) ) ;
#7153 = CARTESIAN_POINT ( 'NONE',  ( -14.40394475573011945, -10.79473832354794283, -3.799999999999999822 ) ) ;
#7154 = CARTESIAN_POINT ( 'NONE',  ( 85.79342132543153809, 17.83186255874426962, 7.000000000000000000 ) ) ;
#7155 = LINE ( 'NONE', #9534, #9434 ) ;
#7156 = EDGE_CURVE ( 'NONE', #14360, #10918, #9751, .T. ) ;
#7157 = B_SPLINE_CURVE_WITH_KNOTS ( 'NONE', 3,
 ( #5055, #11944, #1736, #1660, #563, #6122, #1433, #2739 ),
 .UNSPECIFIED., .F., .F.,
 ( 4, 2, 2, 4 ),
 ( 1.984117563342667082E-07, 0.001895214258086352519, 0.002842722181251361793, 0.003790230104416370850 ),
 .UNSPECIFIED. ) ;
#7158 = CARTESIAN_POINT ( 'NONE',  ( 0.7686372430964689695, -4.022333916463475489, -17.00993931356764932 ) ) ;
#7159 = ORIENTED_EDGE ( 'NONE', *, *, #5267, .T. ) ;
#7160 = CARTESIAN_POINT ( 'NONE',  ( 65.94650549498813064, -33.90026220706954518, 6.000000000000000000 ) ) ;
#7161 = VECTOR ( 'NONE', #14753, 1000.000000000000114 ) ;
#7162 = ORIENTED_EDGE ( 'NONE', *, *, #12918, .F. ) ;
#7163 = LINE ( 'NONE', #7242, #10446 ) ;
#7164 = DIRECTION ( 'NONE',  ( 0.000000000000000000, 0.000000000000000000, 1.000000000000000000 ) ) ;
#7165 = ADVANCED_FACE ( 'NONE', ( #8737 ), #13433, .F. ) ;
#7166 = VERTEX_POINT ( 'NONE', #3060 ) ;
#7167 = VERTEX_POINT ( 'NONE', #12431 ) ;
#7168 = DIRECTION ( 'NONE',  ( 0.000000000000000000, -1.000000000000000000, 0.000000000000000000 ) ) ;
#7169 = ORIENTED_EDGE ( 'NONE', *, *, #9165, .F. ) ;
#7170 = AXIS2_PLACEMENT_3D ( 'NONE', #2507, #9352, #4680 ) ;
#7171 = CYLINDRICAL_SURFACE ( 'NONE', #2570, 8.400000000000000355 ) ;
#7172 = CARTESIAN_POINT ( 'NONE',  ( -5.999999999999999112, 0.000000000000000000, 3.895000000000000462 ) ) ;
#7173 = ADVANCED_FACE ( 'NONE', ( #10348 ), #5605, .F. ) ;
#7174 = CARTESIAN_POINT ( 'NONE',  ( -18.40394475573011945, -10.79473832354794460, -3.799999999999999378 ) ) ;
#7175 = CARTESIAN_POINT ( 'NONE',  ( 0.000000000000000000, 0.000000000000000000, 0.000000000000000000 ) ) ;
#7176 = B_SPLINE_CURVE_WITH_KNOTS ( 'NONE', 3,
 ( #13959, #4898, #10574, #8401 ),
 .UNSPECIFIED., .F., .F.,
 ( 4, 4 ),
 ( 1.981826382900849143E-07, 0.0006887856082032019125 ),
 .UNSPECIFIED. ) ;
#7177 = VERTEX_POINT ( 'NONE', #10280 ) ;
#7178 = LINE ( 'NONE', #6881, #2282 ) ;
#7179 = ADVANCED_FACE ( 'NONE', ( #9202 ), #13659, .F. ) ;
#7180 = CARTESIAN_POINT ( 'NONE',  ( 2.789999999999999147, 1.621424371464993087E-13, -12.95481323787947936 ) ) ;
#7181 = ORIENTED_EDGE ( 'NONE', *, *, #10529, .T. ) ;
#7182 = AXIS2_PLACEMENT_3D ( 'NONE', #2226, #4758, #10528 ) ;
#7183 = ORIENTED_EDGE ( 'NONE', *, *, #11956, .F. ) ;
#7184 = VERTEX_POINT ( 'NONE', #1910 ) ;
#7185 = CARTESIAN_POINT ( 'NONE',  ( 0.02436607992776411782, -16.37294372382844543, -18.55949924794910544 ) ) ;
#7186 = DIRECTION ( 'NONE',  ( 0.000000000000000000, 0.000000000000000000, 1.000000000000000000 ) ) ;
#7187 = CARTESIAN_POINT ( 'NONE',  ( 2.789999999999999147, 9.324097380959765147, -22.25075486061728824 ) ) ;
#7188 = FACE_OUTER_BOUND ( 'NONE', #12481, .T. ) ;
#7189 = DIRECTION ( 'NONE',  ( -1.000000000000000000, 0.000000000000000000, 0.000000000000000000 ) ) ;
#7190 = DIRECTION ( 'NONE',  ( -1.000000000000000000, -0.000000000000000000, -0.000000000000000000 ) ) ;
#7191 = ADVANCED_FACE ( 'NONE', ( #14898 ), #9129, .F. ) ;
#7192 = ORIENTED_EDGE ( 'NONE', *, *, #7835, .F. ) ;
#7193 = LINE ( 'NONE', #1346, #6344 ) ;
#7194 = CARTESIAN_POINT ( 'NONE',  ( 0.7592463965288823724, -12.98165646470099155, 24.32906614999610895 ) ) ;
#7195 = CARTESIAN_POINT ( 'NONE',  ( 0.07181524296601451973, 16.91181672897733534, 18.89296398180198011 ) ) ;
#7196 = FACE_OUTER_BOUND ( 'NONE', #4822, .T. ) ;
#7197 = ORIENTED_EDGE ( 'NONE', *, *, #1768, .T. ) ;
#7198 = ORIENTED_EDGE ( 'NONE', *, *, #6649, .T. ) ;
#7199 = ADVANCED_FACE ( 'NONE', ( #13810, #6516 ), #8969, .T. ) ;
#7200 = ORIENTED_EDGE ( 'NONE', *, *, #7892, .T. ) ;
#7201 = CARTESIAN_POINT ( 'NONE',  ( 2.715264245299032986, 11.74839219818101910, -9.749517823373880177 ) ) ;
#7202 = DIRECTION ( 'NONE',  ( -0.000000000000000000, -0.000000000000000000, 1.000000000000000000 ) ) ;
#7203 = CARTESIAN_POINT ( 'NONE',  ( 2.789999999999999147, -13.40591150984221080, -5.214906618939850524 ) ) ;
#7204 = CARTESIAN_POINT ( 'NONE',  ( 2.765633920072235963, -16.37294372382871188, 18.55949924794887096 ) ) ;
#7205 = DIRECTION ( 'NONE',  ( 0.000000000000000000, 0.000000000000000000, -1.000000000000000000 ) ) ;
#7206 = DIRECTION ( 'NONE',  ( -1.000000000000000000, -0.000000000000000000, -0.000000000000000000 ) ) ;
#7207 = EDGE_LOOP ( 'NONE', ( #3092, #13599, #596, #2578, #7023, #12724, #6717, #1682, #3617, #10173 ) ) ;
#7208 = DIRECTION ( 'NONE',  ( -1.000000000000000000, 0.000000000000000000, 0.000000000000000000 ) ) ;
#7209 = CARTESIAN_POINT ( 'NONE',  ( 8.000000000000000000, 0.000000000000000000, 0.000000000000000000 ) ) ;
#7210 = EDGE_CURVE ( 'NONE', #10832, #8536, #8089, .T. ) ;
#7211 = ADVANCED_FACE ( 'NONE', ( #1989 ), #6673, .F. ) ;
#7212 = AXIS2_PLACEMENT_3D ( 'NONE', #9969, #12424, #3979 ) ;
#7213 = ORIENTED_EDGE ( 'NONE', *, *, #9029, .F. ) ;
#7214 = FACE_OUTER_BOUND ( 'NONE', #6160, .T. ) ;
#7215 = DIRECTION ( 'NONE',  ( 5.480158469902919838E-17, 1.051478716308701618E-16, 1.000000000000000000 ) ) ;
#7216 = CLOSED_SHELL ( 'NONE', ( #4014, #2208, #9609, #252, #1949, #7040 ) ) ;
#7217 = DIRECTION ( 'NONE',  ( 0.000000000000000000, 0.000000000000000000, 1.000000000000000000 ) ) ;
#7218 = ORIENTED_EDGE ( 'NONE', *, *, #12503, .T. ) ;
#7219 = CIRCLE ( 'NONE', #10168, 6.000000000000000000 ) ;
#7220 = AXIS2_PLACEMENT_3D ( 'NONE', #2686, #583, #9594 ) ;
#7221 = ORIENTED_EDGE ( 'NONE', *, *, #8336, .T. ) ;
#7222 = ORIENTED_EDGE ( 'NONE', *, *, #3938, .T. ) ;
#7223 = ORIENTED_EDGE ( 'NONE', *, *, #5242, .F. ) ;
#7224 = CARTESIAN_POINT ( 'NONE',  ( 0.1438988480186108865, -14.59528211759996630, 5.279841123860814278 ) ) ;
#7225 = CARTESIAN_POINT ( 'NONE',  ( 2.765633920072233742, -24.15498966839966855, 5.391175441198523544 ) ) ;
#7226 = CARTESIAN_POINT ( 'NONE',  ( 2.789999999999999147, 13.87420763704361093, -1.948757464274220697 ) ) ;
#7227 = CARTESIAN_POINT ( 'NONE',  ( 2.765633920072241292, 18.55949924794916228, -16.37294372382838148 ) ) ;
#7228 = ADVANCED_FACE ( 'NONE', ( #11349 ), #11198, .T. ) ;
#7229 = CIRCLE ( 'NONE', #854, 5.999999999999999112 ) ;
#7230 = EDGE_CURVE ( 'NONE', #2043, #4505, #3283, .T. ) ;
#7232 = COLOUR_RGB ( '',1.000000000000000000, 0.9490196078431372140, 0.9098039215686274384 ) ;
#7231 = CARTESIAN_POINT ( 'NONE',  ( 0.07473579423048611059, -2.569134216959001904, 15.04916547791953541 ) ) ;
#7233 = EDGE_CURVE ( 'NONE', #3010, #852, #4370, .T. ) ;
#7234 = VERTEX_POINT ( 'NONE', #9056 ) ;
#7235 = DIRECTION ( 'NONE',  ( 5.480158469902919838E-17, 1.051478716308701618E-16, 1.000000000000000000 ) ) ;
#7236 = AXIS2_PLACEMENT_3D ( 'NONE', #2431, #11716, #5896 ) ;
#7237 = CIRCLE ( 'NONE', #4552, 24.12539914357697768 ) ;
#7238 = ADVANCED_FACE ( 'NONE', ( #3360 ), #4889, .T. ) ;
#7239 = VECTOR ( 'NONE', #3763, 1000.000000000000227 ) ;
#7240 =( REPRESENTATION_RELATIONSHIP ('NONE','NONE', #12685, #7313 ) REPRESENTATION_RELATIONSHIP_WITH_TRANSFORMATION ( #10197 )SHAPE_REPRESENTATION_RELATIONSHIP( ) );
#7241 = VERTEX_POINT ( 'NONE', #5386 ) ;
#7242 = CARTESIAN_POINT ( 'NONE',  ( -0.1374368770859596967, -4.808326913195983821, -0.8000000000000000444 ) ) ;
#7243 = CARTESIAN_POINT ( 'NONE',  ( 2.789999999999999147, 7.334849878007844382, -23.31896751603323992 ) ) ;
#7244 = ORIENTED_EDGE ( 'NONE', *, *, #13068, .T. ) ;
#7245 = ORIENTED_EDGE ( 'NONE', *, *, #2735, .F. ) ;
#7246 = CARTESIAN_POINT ( 'NONE',  ( 0.000000000000000000, -11.04103753892265871, -8.624777288397922348 ) ) ;
#7247 = AXIS2_PLACEMENT_3D ( 'NONE', #14649, #13323, #9949 ) ;
#7248 = VERTEX_POINT ( 'NONE', #975 ) ;
#7249 = AXIS2_PLACEMENT_3D ( 'NONE', #13380, #3942, #384 ) ;
#7250 = AXIS2_PLACEMENT_3D ( 'NONE', #13697, #5781, #10460 ) ;
#7251 = DIRECTION ( 'NONE',  ( 5.339417856040273846E-17, 1.063174570779084847E-17, -1.000000000000000000 ) ) ;
#7252 = CARTESIAN_POINT ( 'NONE',  ( 0.000000000000000000, 0.000000000000000000, 6.000000000000000000 ) ) ;
#7253 = DIRECTION ( 'NONE',  ( 0.1643989873053574580, -0.9863939238321436376, 0.000000000000000000 ) ) ;
#7254 = DIRECTION ( 'NONE',  ( 1.000000000000000000, 0.000000000000000000, 0.000000000000000000 ) ) ;
#7255 = ORIENTED_EDGE ( 'NONE', *, *, #7758, .F. ) ;
#7256 = CARTESIAN_POINT ( 'NONE',  ( 61.98919079003883326, 3.953582723775848962, -2.000000000000000888 ) ) ;
#7257 = CARTESIAN_POINT ( 'NONE',  ( 0.7686372158811279887, 12.71987259277452154, -11.98841295390584705 ) ) ;
#7258 = VERTEX_POINT ( 'NONE', #2052 ) ;
#7259 = B_SPLINE_CURVE_WITH_KNOTS ( 'NONE', 3,
 ( #5523, #2050, #10122, #9053, #9973, #4446 ),
 .UNSPECIFIED., .F., .F.,
 ( 4, 2, 4 ),
 ( 2.032124546189838441E-07, 0.001878594002992310316, 0.003756984793530001362 ),
 .UNSPECIFIED. ) ;
#7260 = CARTESIAN_POINT ( 'NONE',  ( 1.039999999999996705, 27.76164181293051669, -4.147968289691385202 ) ) ;
#7261 = TOROIDAL_SURFACE ( 'NONE', #15125, 24.12539914357697413, 8.000000000000000000 ) ;
#7262 = ORIENTED_EDGE ( 'NONE', *, *, #1654, .F. ) ;
#7263 = EDGE_LOOP ( 'NONE', ( #14601, #14882, #13075, #3839 ) ) ;
#7264 = DIRECTION ( 'NONE',  ( -1.000000000000000000, 0.000000000000000000, 0.000000000000000000 ) ) ;
#7265 = CARTESIAN_POINT ( 'NONE',  ( 1.394999999999999574, 12.52377138324259676, -25.12109765559640451 ) ) ;
#7266 = CYLINDRICAL_SURFACE ( 'NONE', #8774, 28.06981291497571362 ) ;
#7267 = CARTESIAN_POINT ( 'NONE',  ( 1.039999999999996927, 4.633866840649313090, -27.68468304288253634 ) ) ;
#7268 = DIRECTION ( 'NONE',  ( 1.000000000000000000, 0.000000000000000000, 0.000000000000000000 ) ) ;
#7269 = PRODUCT_DEFINITION_SHAPE ( 'NONE', 'NONE',  #12917 ) ;
#7270 = EDGE_CURVE ( 'NONE', #3390, #2825, #8076, .T. ) ;
#7271 = FACE_OUTER_BOUND ( 'NONE', #906, .T. ) ;
#7272 = VERTEX_POINT ( 'NONE', #12648 ) ;
#7273 = CARTESIAN_POINT ( 'NONE',  ( 2.790000000000000924, 0.000000000000000000, 4.000000000000000000 ) ) ;
#7274 = DIRECTION ( 'NONE',  ( 0.000000000000000000, 0.000000000000000000, 1.000000000000000000 ) ) ;
#7275 = DIRECTION ( 'NONE',  ( -0.000000000000000000, -0.000000000000000000, -1.000000000000000000 ) ) ;
#7276 = CARTESIAN_POINT ( 'NONE',  ( -20.63749999999999574, 0.000000000000000000, 0.000000000000000000 ) ) ;
#7277 = ORIENTED_EDGE ( 'NONE', *, *, #11338, .T. ) ;
#7278 = VERTEX_POINT ( 'NONE', #6819 ) ;
#7279 = AXIS2_PLACEMENT_3D ( 'NONE', #12299, #2849, #12368 ) ;
#7280 = EDGE_LOOP ( 'NONE', ( #6203, #11454 ) ) ;
#7281 = CYLINDRICAL_SURFACE ( 'NONE', #2393, 13.20000000000000284 ) ;
#7282 = CIRCLE ( 'NONE', #3355, 4.000000000000000000 ) ;
#7283 = CYLINDRICAL_SURFACE ( 'NONE', #3618, 4.000000000000000888 ) ;
#7284 = DIRECTION ( 'NONE',  ( 0.000000000000000000, 0.000000000000000000, 1.000000000000000000 ) ) ;
#7285 = AXIS2_PLACEMENT_3D ( 'NONE', #9797, #13074, #10793 ) ;
#7286 = DIRECTION ( 'NONE',  ( -1.000000000000000000, 0.000000000000000000, -0.000000000000000000 ) ) ;
#7287 = DIRECTION ( 'NONE',  ( 0.000000000000000000, 0.000000000000000000, 1.000000000000000000 ) ) ;
#7288 = CARTESIAN_POINT ( 'NONE',  ( 3.799999999999999378, 0.000000000000000000, -0.8000000000000000444 ) ) ;
#7289 = EDGE_CURVE ( 'NONE', #6156, #13028, #8799, .T. ) ;
#7290 = ORIENTED_EDGE ( 'NONE', *, *, #6891, .T. ) ;
#7291 = FACE_OUTER_BOUND ( 'NONE', #128, .T. ) ;
#7292 = CARTESIAN_POINT ( 'NONE',  ( 0.1438988480159978933, 14.59528211758547478, 5.279841123860917307 ) ) ;
#7293 = ORIENTED_EDGE ( 'NONE', *, *, #8775, .F. ) ;
#7295 = AXIS2_PLACEMENT_3D ( 'NONE', #7363, #10808, #263 ) ;
#7294 = DIRECTION ( 'NONE',  ( 1.576560579138138762E-17, -1.359337748750801608E-17, 1.000000000000000000 ) ) ;
#7296 = DIRECTION ( 'NONE',  ( -1.000000000000000000, -0.000000000000000000, -0.000000000000000000 ) ) ;
#7297 = EDGE_CURVE ( 'NONE', #2515, #10827, #11723, .T. ) ;
#7298 = DIRECTION ( 'NONE',  ( 1.000000000000000000, 1.445602896647338917E-16, 0.000000000000000000 ) ) ;
#7299 = VERTEX_POINT ( 'NONE', #9500 ) ;
#7300 = CIRCLE ( 'NONE', #9739, 2.999999999999988898 ) ;
#7301 = CIRCLE ( 'NONE', #9264, 28.06981291497571362 ) ;
#7302 = CARTESIAN_POINT ( 'NONE',  ( 2.764680872515351329, 14.46287784598617421, -2.311161484776606212 ) ) ;
#7303 = CIRCLE ( 'NONE', #14429, 4.000000000000003553 ) ;
#7304 = ORIENTED_EDGE ( 'NONE', *, *, #9473, .F. ) ;
#7305 = ORIENTED_EDGE ( 'NONE', *, *, #4714, .F. ) ;
#7306 = ORIENTED_EDGE ( 'NONE', *, *, #5247, .F. ) ;
#7307 = CARTESIAN_POINT ( 'NONE',  ( 0.4472135954999577612, 0.000000000000000000, 0.000000000000000000 ) ) ;
#7308 = PRODUCT_RELATED_PRODUCT_CATEGORY ( 'part', '', ( #2824 ) ) ;
#7309 = CARTESIAN_POINT ( 'NONE',  ( 0.02531912748606271468, -5.229914364928256454, -13.68080036884353845 ) ) ;
#7310 = ADVANCED_FACE ( 'NONE', ( #10511 ), #9351, .T. ) ;
#7311 = ADVANCED_FACE ( 'NONE', ( #2437, #2211 ), #1130, .F. ) ;
#7312 = CARTESIAN_POINT ( 'NONE',  ( 15.21482963846748504, 16.90833299098317610, 6.000000000000005329 ) ) ;
#7313 = SHAPE_REPRESENTATION ( 'angular contact ball bearing_68_iso_ISO 15 ABB - 178 - 20,SI,NC,20_68', ( #1376 ), #4341 ) ;
#7314 = CARTESIAN_POINT ( 'NONE',  ( -10.00000000000000000, 0.000000000000000000, 0.000000000000000000 ) ) ;
#7315 = DIRECTION ( 'NONE',  ( 1.000000000000000000, 0.000000000000000000, 0.000000000000000000 ) ) ;
#7316 = PRESENTATION_LAYER_ASSIGNMENT (  '', '', ( #1413 ) ) ;
#7317 = CARTESIAN_POINT ( 'NONE',  ( 5.999999999999999112, 7.347880794884118750E-16, 5.500000000000000000 ) ) ;
#7318 = EDGE_LOOP ( 'NONE', ( #5064, #5170 ) ) ;
#7319 = AXIS2_PLACEMENT_3D ( 'NONE', #1673, #6358, #11041 ) ;
#7320 = DIRECTION ( 'NONE',  ( -0.000000000000000000, -0.000000000000000000, 1.000000000000000000 ) ) ;
#7321 = AXIS2_PLACEMENT_3D ( 'NONE', #6783, #11966, #4764 ) ;
#7322 = EDGE_CURVE ( 'NONE', #7692, #851, #3167, .T. ) ;
#7323 = B_SPLINE_CURVE_WITH_KNOTS ( 'NONE', 3,
 ( #2737, #9576, #10728, #10803 ),
 .UNSPECIFIED., .F., .F.,
 ( 4, 4 ),
 ( 2.034713381942770033E-07, 0.0006045424356928436873 ),
 .UNSPECIFIED. ) ;
#7324 = TOROIDAL_SURFACE ( 'NONE', #7067, 24.12539914357697413, 8.000000000000000000 ) ;
#7325 = ORIENTED_EDGE ( 'NONE', *, *, #4041, .T. ) ;
#7326 = VERTEX_POINT ( 'NONE', #6965 ) ;
#7327 = CARTESIAN_POINT ( 'NONE',  ( -10.00000000000000000, 0.000000000000000000, 0.000000000000000000 ) ) ;
#7328 = LINE ( 'NONE', #6163, #9947 ) ;
#7329 = ADVANCED_FACE ( 'NONE', ( #31, #2355 ), #11645, .T. ) ;
#7330 = VERTEX_POINT ( 'NONE', #12867 ) ;
#7331 = ORIENTED_EDGE ( 'NONE', *, *, #8973, .F. ) ;
#7332 = CIRCLE ( 'NONE', #1431, 2.524999999999995914 ) ;
#7333 = B_SPLINE_CURVE_WITH_KNOTS ( 'NONE', 3,
 ( #8400, #6114, #8706, #13400 ),
 .UNSPECIFIED., .F., .F.,
 ( 4, 4 ),
 ( 2.135345996175579449E-07, 0.0006888010880210803950 ),
 .UNSPECIFIED. ) ;
#7334 = CYLINDRICAL_SURFACE ( 'NONE', #5316, 3.799999999999999378 ) ;
#7335 = ADVANCED_FACE ( 'NONE', ( #5900 ), #8189, .F. ) ;
#7336 = VERTEX_POINT ( 'NONE', #9413 ) ;
#7337 = CARTESIAN_POINT ( 'NONE',  ( 33.82574562093736859, -6.697933970950280091, 7.000000000000000000 ) ) ;
#7338 = DIRECTION ( 'NONE',  ( 0.000000000000000000, 0.000000000000000000, 1.000000000000000000 ) ) ;
#7339 = CARTESIAN_POINT ( 'NONE',  ( 0.02436607992776541887, 12.59161484032942901, -21.30679549418617924 ) ) ;
#7340 = CARTESIAN_POINT ( 'NONE',  ( 2.031033465052725084, -27.14933624560904946, -4.828387785248313691 ) ) ;
#7341 = VECTOR ( 'NONE', #14143, 1000.000000000000000 ) ;
#7342 = ORIENTED_EDGE ( 'NONE', *, *, #11881, .F. ) ;
#7343 = AXIS2_PLACEMENT_3D ( 'NONE', #12794, #3659, #2506 ) ;
#7344 = CARTESIAN_POINT ( 'NONE',  ( 2.030753605846574494, 3.797885586973597682, -27.31305418910206129 ) ) ;
#7345 = CARTESIAN_POINT ( 'NONE',  ( 2.790000000000000036, 0.000000000000000000, 0.000000000000000000 ) ) ;
#7346 = ORIENTED_EDGE ( 'NONE', *, *, #2054, .T. ) ;
#7347 = CARTESIAN_POINT ( 'NONE',  ( 1.039999999999996261, 12.83329210556831512, 12.55714665599991697 ) ) ;
#7348 = B_SPLINE_CURVE_WITH_KNOTS ( 'NONE', 3,
 ( #8658, #7447, #13274, #11964 ),
 .UNSPECIFIED., .F., .F.,
 ( 4, 4 ),
 ( 2.324263106244698315E-07, 0.0006888201370294677779 ),
 .UNSPECIFIED. ) ;
#7349 = ORIENTED_EDGE ( 'NONE', *, *, #612, .T. ) ;
#7350 = EDGE_LOOP ( 'NONE', ( #13693, #12874, #8130, #11051 ) ) ;
#7351 = CARTESIAN_POINT ( 'NONE',  ( 2.789679245949062913, -20.70663861606260525, -12.51925356660783528 ) ) ;
#7352 = CARTESIAN_POINT ( 'NONE',  ( 2.789999999999999147, 24.34211360614300190, 7.909232158574900140 ) ) ;
#7353 = CARTESIAN_POINT ( 'NONE',  ( 0.000000000000000000, 0.000000000000000000, 0.000000000000000000 ) ) ;
#7354 = CARTESIAN_POINT ( 'NONE',  ( 2.262072625383131363, 26.57710921259761960, 4.996265754456460151 ) ) ;
#7355 = ITEM_DEFINED_TRANSFORMATION ( 'NONE', 'NONE', #14619,  #1376 ) ;
#7357 = AXIS2_PLACEMENT_3D ( 'NONE', #4143, #3054, #4365 ) ;
#7356 = LINE ( 'NONE', #10727, #1954 ) ;
#7358 = CARTESIAN_POINT ( 'NONE',  ( 88.46153288930041469, 16.46030115554384565, -2.000000000000000888 ) ) ;
#7359 = ORIENTED_EDGE ( 'NONE', *, *, #5219, .T. ) ;
#7360 = DIRECTION ( 'NONE',  ( -0.9728364810787193395, -0.2314933715733012709, 0.000000000000000000 ) ) ;
#7361 = CARTESIAN_POINT ( 'NONE',  ( 32.66827876307085887, -1.833751565556681173, 7.000000000000000000 ) ) ;
#7362 = DIRECTION ( 'NONE',  ( 1.000000000000000000, 0.000000000000000000, 0.000000000000000000 ) ) ;
#7363 = CARTESIAN_POINT ( 'NONE',  ( 0.000000000000000000, 15.47981323787947794, 0.000000000000000000 ) ) ;
#7364 = ORIENTED_EDGE ( 'NONE', *, *, #12758, .T. ) ;
#7365 = CIRCLE ( 'NONE', #730, 24.12539914357697768 ) ;
#7366 = ORIENTED_EDGE ( 'NONE', *, *, #2598, .T. ) ;
#7367 = ORIENTED_EDGE ( 'NONE', *, *, #2860, .F. ) ;
#7368 = CARTESIAN_POINT ( 'NONE',  ( -14.40394475573011945, -10.79473832354794460, -5.000000000000000000 ) ) ;
#7369 = CARTESIAN_POINT ( 'NONE',  ( 2.789999999999999147, 5.391175441198615914, 24.15498966839965078 ) ) ;
#7370 = EDGE_CURVE ( 'NONE', #8417, #5700, #14109, .T. ) ;
#7371 = CARTESIAN_POINT ( 'NONE',  ( 2.765633920072236851, -22.71065055754445439, -9.836394144775947979 ) ) ;
#7372 = CARTESIAN_POINT ( 'NONE',  ( -1.249999999999997558, 0.000000000000000000, 0.000000000000000000 ) ) ;
#7373 = DIRECTION ( 'NONE',  ( 0.000000000000000000, 0.000000000000000000, 1.000000000000000000 ) ) ;
#7374 = DIRECTION ( 'NONE',  ( -0.000000000000000000, -0.000000000000000000, -1.000000000000000000 ) ) ;
#7375 = ORIENTED_EDGE ( 'NONE', *, *, #6823, .T. ) ;
#7376 = CARTESIAN_POINT ( 'NONE',  ( -4.000000000000000000, 0.000000000000000000, 3.895000000000000462 ) ) ;
#7377 = CARTESIAN_POINT ( 'NONE',  ( -16.23224367729419271, -7.237025146040845236, -3.800000000000000266 ) ) ;
#7378 = AXIS2_PLACEMENT_3D ( 'NONE', #12967, #2456, #7140 ) ;
#7379 = ORIENTED_EDGE ( 'NONE', *, *, #15025, .T. ) ;
#7380 = CARTESIAN_POINT ( 'NONE',  ( 93.49175023922396122, 0.6585002008270834928, 2.999999999999999112 ) ) ;
#7381 = CARTESIAN_POINT ( 'NONE',  ( 2.030753602223784871, 27.14986936243581184, -4.828194074574073902 ) ) ;
#7382 = CARTESIAN_POINT ( 'NONE',  ( 1.960886852992497653, -24.44424927289185590, 12.96989951879399072 ) ) ;
#7383 = EDGE_CURVE ( 'NONE', #14623, #3735, #11985, .T. ) ;
#7384 = ORIENTED_EDGE ( 'NONE', *, *, #2116, .T. ) ;
#7385 = EDGE_CURVE ( 'NONE', #8382, #12063, #4611, .T. ) ;
#7386 = CARTESIAN_POINT ( 'NONE',  ( 0.000000000000000000, 12.98979500319701685, -5.249430348645618416 ) ) ;
#7387 = LINE ( 'NONE', #7455, #12413 ) ;
#7388 = VERTEX_POINT ( 'NONE', #12948 ) ;
#7389 = ORIENTED_EDGE ( 'NONE', *, *, #8095, .F. ) ;
#7390 = ORIENTED_EDGE ( 'NONE', *, *, #14242, .F. ) ;
#7391 = CARTESIAN_POINT ( 'NONE',  ( 2.789999999999999147, -9.324097380959294412, -22.25075486061747654 ) ) ;
#7392 = CARTESIAN_POINT ( 'NONE',  ( 1.394999999999998685, -27.76164181293049182, -4.147968289691579713 ) ) ;
#7393 = EDGE_CURVE ( 'NONE', #5234, #7126, #13963, .T. ) ;
#7394 = CARTESIAN_POINT ( 'NONE',  ( 2.789999999999999147, -5.249430348645846678, 12.98979500319692448 ) ) ;
#7395 = CARTESIAN_POINT ( 'NONE',  ( 2.740003288479520904, -2.439987328297072544, 14.75565684666126387 ) ) ;
#7396 = LINE ( 'NONE', #5014, #14092 ) ;
#7397 = ORIENTED_EDGE ( 'NONE', *, *, #13281, .F. ) ;
#7398 = CARTESIAN_POINT ( 'NONE',  ( -4.000000000000000000, 0.000000000000000000, 4.000000000000000000 ) ) ;
#7399 = EDGE_CURVE ( 'NONE', #8616, #8417, #6959, .T. ) ;
#7400 = VERTEX_POINT ( 'NONE', #14267 ) ;
#7401 = EDGE_LOOP ( 'NONE', ( #11031, #1414, #9162, #12268 ) ) ;
#7402 = CYLINDRICAL_SURFACE ( 'NONE', #11660, 17.95481323787947403 ) ;
#7403 = PLANE ( 'NONE',  #361 ) ;
#7404 = VERTEX_POINT ( 'NONE', #6894 ) ;
#7405 = ADVANCED_FACE ( 'NONE', ( #1050 ), #5745, .T. ) ;
#7406 = CARTESIAN_POINT ( 'NONE',  ( -9.403944755730119454, -4.794738323547945491, 22.00000000000000000 ) ) ;
#7407 = EDGE_CURVE ( 'NONE', #7557, #13658, #7193, .T. ) ;
#7408 = ORIENTED_EDGE ( 'NONE', *, *, #11141, .F. ) ;
#7409 = DIRECTION ( 'NONE',  ( -0.000000000000000000, -0.000000000000000000, 1.000000000000000000 ) ) ;
#7410 = CARTESIAN_POINT ( 'NONE',  ( 2.789999999999999147, -7.909232158574647009, -24.34211360614308006 ) ) ;
#7411 = ADVANCED_FACE ( 'NONE', ( #8573 ), #1578, .F. ) ;
#7412 = ADVANCED_FACE ( 'NONE', ( #3728 ), #1505, .T. ) ;
#7413 = LINE ( 'NONE', #4885, #8196 ) ;
#7414 = EDGE_LOOP ( 'NONE', ( #2641, #7816, #9962, #14352, #13554 ) ) ;
#7415 = CARTESIAN_POINT ( 'NONE',  ( 2.789999999999999147, -15.47981323787947794, -1.080949580976661932E-13 ) ) ;
#7416 = PLANE ( 'NONE',  #1155 ) ;
#7417 = ORIENTED_EDGE ( 'NONE', *, *, #5979, .T. ) ;
#7418 = CARTESIAN_POINT ( 'NONE',  ( 2.790000000000000924, 0.000000000000000000, 0.000000000000000000 ) ) ;
#7419 = CARTESIAN_POINT ( 'NONE',  ( 1.749999999999999778, -17.29145405592685236, -4.835383649608663070 ) ) ;
#7420 = ORIENTED_EDGE ( 'NONE', *, *, #660, .F. ) ;
#7421 = EDGE_LOOP ( 'NONE', ( #3258, #6752, #10064, #247 ) ) ;
#7422 = FACE_OUTER_BOUND ( 'NONE', #10294, .T. ) ;
#7423 = CARTESIAN_POINT ( 'NONE',  ( 2.604434514863827488, -10.67816411292148793, -23.63475234378993761 ) ) ;
#7424 = B_SPLINE_CURVE_WITH_KNOTS ( 'NONE', 3,
 ( #14413, #9291, #3442, #12803 ),
 .UNSPECIFIED., .F., .F.,
 ( 4, 4 ),
 ( 1.984117563342612819E-07, 0.0009182716802119580664 ),
 .UNSPECIFIED. ) ;
#7425 = EDGE_CURVE ( 'NONE', #3101, #9188, #5135, .T. ) ;
#7426 = FACE_OUTER_BOUND ( 'NONE', #7003, .T. ) ;
#7427 = B_SPLINE_CURVE_WITH_KNOTS ( 'NONE', 3,
 ( #11830, #63, #9381, #3765, #4863, #8450, #2623, #1306 ),
 .UNSPECIFIED., .F., .F.,
 ( 4, 2, 2, 4 ),
 ( 4.663089536307126026E-07, 0.001898630414085407782, 0.002847712466651296237, 0.003796794519217184909 ),
 .UNSPECIFIED. ) ;
#7429 = ORIENTED_EDGE ( 'NONE', *, *, #4240, .F. ) ;
#7428 = ADVANCED_FACE ( 'NONE', ( #3967 ), #13090, .T. ) ;
#7430 = DIRECTION ( 'NONE',  ( -1.000000000000000000, -0.000000000000000000, -0.000000000000000000 ) ) ;
#7431 = DIRECTION ( 'NONE',  ( 0.1305261922200521840, 0.9914448613738103822, -0.000000000000000000 ) ) ;
#7432 = FACE_OUTER_BOUND ( 'NONE', #10182, .T. ) ;
#7433 = SURFACE_STYLE_USAGE ( .BOTH. , #3970 ) ;
#7434 = VECTOR ( 'NONE', #10818, 1000.000000000000000 ) ;
#7435 = EDGE_LOOP ( 'NONE', ( #7644, #7998, #2760, #8050, #3040 ) ) ;
#7436 = VERTEX_POINT ( 'NONE', #12096 ) ;
#7437 = EDGE_CURVE ( 'NONE', #3359, #12316, #412, .T. ) ;
#7438 = ORIENTED_EDGE ( 'NONE', *, *, #4586, .F. ) ;
#7439 = DIRECTION ( 'NONE',  ( 0.000000000000000000, 0.000000000000000000, 1.000000000000000000 ) ) ;
#7440 = CARTESIAN_POINT ( 'NONE',  ( 2.604434325169353581, -2.851997810081467577, -25.77772010606609498 ) ) ;
#7441 = CARTESIAN_POINT ( 'NONE',  ( 83.50748565343083385, 13.38500995229612478, 7.000000000000000000 ) ) ;
#7442 = CARTESIAN_POINT ( 'NONE',  ( 80.00000000000000000, 1.084202172485504434E-16, 8.673617379884035472E-15 ) ) ;
#7443 = CARTESIAN_POINT ( 'NONE',  ( 1.749999999999999778, 17.29145405592688789, 4.835383649608534284 ) ) ;
#7444 = VECTOR ( 'NONE', #6025, 1000.000000000000000 ) ;
#7445 = ORIENTED_EDGE ( 'NONE', *, *, #4217, .T. ) ;
#7446 = FACE_OUTER_BOUND ( 'NONE', #5725, .T. ) ;
#7447 = CARTESIAN_POINT ( 'NONE',  ( 0.006974693931641778172, 18.43727551351055283, -16.17543236987968669 ) ) ;
#7448 = ORIENTED_EDGE ( 'NONE', *, *, #14334, .T. ) ;
#7449 = DIRECTION ( 'NONE',  ( -1.000000000000000000, 0.000000000000000000, 0.000000000000000000 ) ) ;
#7450 = DIRECTION ( 'NONE',  ( 0.000000000000000000, 0.000000000000000000, -1.000000000000000000 ) ) ;
#7451 = CARTESIAN_POINT ( 'NONE',  ( 2.030753610301984313, -19.12676442129359700, 19.86438386685654578 ) ) ;
#7452 = ORIENTED_EDGE ( 'NONE', *, *, #7600, .F. ) ;
#7453 = B_SPLINE_CURVE_WITH_KNOTS ( 'NONE', 3,
 ( #10583, #7194, #8190, #12868, #1207, #11573 ),
 .UNSPECIFIED., .F., .F.,
 ( 4, 2, 4 ),
 ( 4.462636695653741059E-07, 0.001879885036799761782, 0.003759323809929957915 ),
 .UNSPECIFIED. ) ;
#7454 = CARTESIAN_POINT ( 'NONE',  ( -16.64001273322991281, -4.794738323547945491, 14.99999999999999822 ) ) ;
#7455 = CARTESIAN_POINT ( 'NONE',  ( -9.999999999999998224, 0.000000000000000000, -130.1575142076926852 ) ) ;
#7456 = ORIENTED_EDGE ( 'NONE', *, *, #540, .T. ) ;
#7457 = EDGE_LOOP ( 'NONE', ( #10270, #9082, #8879, #7735 ) ) ;
#7458 = ORIENTED_EDGE ( 'NONE', *, *, #12652, .T. ) ;
#7459 = LINE ( 'NONE', #4157, #6801 ) ;
#7460 = DIRECTION ( 'NONE',  ( 1.000000000000000000, 0.000000000000000000, 0.000000000000000000 ) ) ;
#7461 = CARTESIAN_POINT ( 'NONE',  ( 2.604434404052933694, 17.45907811351455408, 19.17825124759784572 ) ) ;
#7462 = CARTESIAN_POINT ( 'NONE',  ( 0.000000000000000000, 20.70663861606293210, -15.04425356660737556 ) ) ;
#7463 = B_SPLINE_CURVE_WITH_KNOTS ( 'NONE', 3,
 ( #4739, #182, #9571, #1340 ),
 .UNSPECIFIED., .F., .F.,
 ( 4, 4 ),
 ( 2.159563976394568454E-07, 0.0006916893629248619269 ),
 .UNSPECIFIED. ) ;
#7464 = DIRECTION ( 'NONE',  ( 0.000000000000000000, 0.000000000000000000, 1.000000000000000000 ) ) ;
#7465 = CARTESIAN_POINT ( 'NONE',  ( 2.262072769566603636, 24.43806413951692136, -11.57956866523193185 ) ) ;
#7466 = EDGE_CURVE ( 'NONE', #6526, #4130, #7824, .T. ) ;
#7467 = ORIENTED_EDGE ( 'NONE', *, *, #12634, .F. ) ;
#7468 = DIRECTION ( 'NONE',  ( -1.000000000000000000, -0.000000000000000000, -0.000000000000000000 ) ) ;
#7469 = AXIS2_PLACEMENT_3D ( 'NONE', #3825, #9827, #7524 ) ;
#7470 = VERTEX_POINT ( 'NONE', #9645 ) ;
#7471 = VERTEX_POINT ( 'NONE', #7273 ) ;
#7472 = LINE ( 'NONE', #6317, #14380 ) ;
#7473 = AXIS2_PLACEMENT_3D ( 'NONE', #9462, #7, #4947 ) ;
#7474 = CARTESIAN_POINT ( 'NONE',  ( 1.039999999999997593, 0.000000000000000000, 0.000000000000000000 ) ) ;
#7475 = ORIENTED_EDGE ( 'NONE', *, *, #2287, .F. ) ;
#7476 = CIRCLE ( 'NONE', #8685, 28.06981291497571007 ) ;
#7477 = UNCERTAINTY_MEASURE_WITH_UNIT (LENGTH_MEASURE( 1.000000000000000082E-05 ), #3886, 'distance_accuracy_value', 'NONE');
#7478 = CARTESIAN_POINT ( 'NONE',  ( -20.63749999999999574, 0.000000000000000000, -6.000000000000001776 ) ) ;
#7479 = VERTEX_POINT ( 'NONE', #7582 ) ;
#7480 = CARTESIAN_POINT ( 'NONE',  ( -1.000000000000000000, -6.008326913195983998, -0.8000000000000000444 ) ) ;
#7481 = CARTESIAN_POINT ( 'NONE',  ( 1.039999999999998925, -4.147968289691484678, 27.76164181293050248 ) ) ;
#7482 = VECTOR ( 'NONE', #11829, 1000.000000000000227 ) ;
#7483 = CIRCLE ( 'NONE', #855, 9.999999999999994671 ) ;
#7484 = DIRECTION ( 'NONE',  ( -0.000000000000000000, -1.000000000000000000, -0.000000000000000000 ) ) ;
#7485 = VECTOR ( 'NONE', #12162, 1000.000000000000000 ) ;
#7486 = EDGE_CURVE ( 'NONE', #12123, #3403, #13211, .T. ) ;
#7487 = B_SPLINE_CURVE_WITH_KNOTS ( 'NONE', 3,
 ( #6280, #9885, #7440, #6359, #5380, #14441 ),
 .UNSPECIFIED., .F., .F.,
 ( 4, 2, 4 ),
 ( 2.132675795048140697E-07, 0.001878604073277005205, 0.003756994878974505639 ),
 .UNSPECIFIED. ) ;
#7488 = PLANE ( 'NONE',  #8865 ) ;
#7489 = DIRECTION ( 'NONE',  ( 0.9148936170212769170, 0.4036950204470268200, -0.000000000000000000 ) ) ;
#7490 = ORIENTED_EDGE ( 'NONE', *, *, #9634, .F. ) ;
#7491 = DIRECTION ( 'NONE',  ( 0.000000000000000000, 0.000000000000000000, -1.000000000000000000 ) ) ;
#7492 = LINE ( 'NONE', #2875, #7485 ) ;
#7493 = AXIS2_PLACEMENT_3D ( 'NONE', #3908, #2750, #10817 ) ;
#7494 = EDGE_LOOP ( 'NONE', ( #1913, #11792 ) ) ;
#7495 = ORIENTED_EDGE ( 'NONE', *, *, #14425, .T. ) ;
#7496 = CARTESIAN_POINT ( 'NONE',  ( -4.000000000000000888, 0.000000000000000000, -7.000000000000007994 ) ) ;
#7498 = DIRECTION ( 'NONE',  ( 0.000000000000000000, 0.000000000000000000, 1.000000000000000000 ) ) ;
#7497 = CIRCLE ( 'NONE', #603, 2.524999999999995914 ) ;
#7499 = ADVANCED_FACE ( 'NONE', ( #14341 ), #11101, .T. ) ;
#7500 = EDGE_CURVE ( 'NONE', #14991, #15036, #9537, .T. ) ;
#7501 = CIRCLE ( 'NONE', #12638, 4.000000000000000000 ) ;
#7502 = CARTESIAN_POINT ( 'NONE',  ( 1.749999999999998002, 27.68468304288259318, 4.633866840649019103 ) ) ;
#7503 = DIRECTION ( 'NONE',  ( -0.000000000000000000, -0.000000000000000000, 1.000000000000000000 ) ) ;
#7504 = ORIENTED_EDGE ( 'NONE', *, *, #8253, .T. ) ;
#7505 = LINE ( 'NONE', #12260, #13463 ) ;
#7506 = CARTESIAN_POINT ( 'NONE',  ( 0.000000000000000000, 1.621424371464993087E-13, -15.47981323787947794 ) ) ;
#7507 = DIRECTION ( 'NONE',  ( 0.000000000000000000, 0.000000000000000000, 1.000000000000000000 ) ) ;
#7508 = FACE_OUTER_BOUND ( 'NONE', #7065, .T. ) ;
#7509 = AXIS2_PLACEMENT_3D ( 'NONE', #11613, #9168, #947 ) ;
#7510 = ORIENTED_EDGE ( 'NONE', *, *, #5362, .F. ) ;
#7511 = EDGE_CURVE ( 'NONE', #4197, #3508, #7505, .T. ) ;
#7512 = ORIENTED_EDGE ( 'NONE', *, *, #2396, .T. ) ;
#7513 = EDGE_CURVE ( 'NONE', #10985, #11120, #7157, .T. ) ;
#7514 = EDGE_LOOP ( 'NONE', ( #10606, #773, #10542, #8889, #7913, #11469 ) ) ;
#7515 = DIRECTION ( 'NONE',  ( 0.000000000000000000, 0.000000000000000000, 1.000000000000000000 ) ) ;
#7516 = CARTESIAN_POINT ( 'NONE',  ( 0.000000000000000000, 0.000000000000000000, 4.500000000000000888 ) ) ;
#7517 = ADVANCED_FACE ( 'NONE', ( #9727 ), #11032, .T. ) ;
#7518 = DIRECTION ( 'NONE',  ( -5.339417856040273846E-17, -1.063174570779084847E-17, 1.000000000000000000 ) ) ;
#7519 = CARTESIAN_POINT ( 'NONE',  ( 0.000000000000000000, 0.000000000000000000, -7.800000000000010481 ) ) ;
#7520 = APPLICATION_PROTOCOL_DEFINITION ( 'draft international standard', 'automotive_design', 1998, #3485 ) ;
#7521 = PLANE ( 'NONE',  #13308 ) ;
#7522 = VECTOR ( 'NONE', #2061, 1000.000000000000000 ) ;
#7523 = CARTESIAN_POINT ( 'NONE',  ( 67.23404255319145761, 28.93147646537026318, -131.1575142076926852 ) ) ;
#7524 = DIRECTION ( 'NONE',  ( 0.000000000000000000, 0.000000000000000000, 1.000000000000000000 ) ) ;
#7525 = ADVANCED_FACE ( 'NONE', ( #6418 ), #1935, .T. ) ;
#7526 = ORIENTED_EDGE ( 'NONE', *, *, #1393, .F. ) ;
#7527 = CARTESIAN_POINT ( 'NONE',  ( 0.02436607992776194942, -5.391175441198450713, -24.15498966839968276 ) ) ;
#7528 = DIRECTION ( 'NONE',  ( 1.000000000000000000, 0.000000000000000000, 0.000000000000000000 ) ) ;
#7529 = DIRECTION ( 'NONE',  ( -0.000000000000000000, -0.000000000000000000, 1.000000000000000000 ) ) ;
#7530 = AXIS2_PLACEMENT_3D ( 'NONE', #14771, #5695, #4394 ) ;
#7531 = ORIENTED_EDGE ( 'NONE', *, *, #14259, .T. ) ;
#7532 = VECTOR ( 'NONE', #8128, 1000.000000000000114 ) ;
#7533 = CARTESIAN_POINT ( 'NONE',  ( 2.740003299868484010, -9.490919315500217834, 11.55877992729661585 ) ) ;
#7534 = DIRECTION ( 'NONE',  ( -1.000000000000000000, 0.000000000000000000, -0.000000000000000000 ) ) ;
#7535 = ORIENTED_EDGE ( 'NONE', *, *, #12170, .F. ) ;
#7536 = TOROIDAL_SURFACE ( 'NONE', #4598, 24.12539914357697768, 8.000000000000000000 ) ;
#7537 = ORIENTED_EDGE ( 'NONE', *, *, #6634, .F. ) ;
#7538 = DIRECTION ( 'NONE',  ( 1.000000000000000000, 0.000000000000000000, 0.000000000000000000 ) ) ;
#7539 = DIRECTION ( 'NONE',  ( 0.000000000000000000, 0.000000000000000000, 1.000000000000000000 ) ) ;
#7540 = B_SPLINE_CURVE_WITH_KNOTS ( 'NONE', 3,
 ( #551, #13315, #9938, #3712 ),
 .UNSPECIFIED., .F., .F.,
 ( 4, 4 ),
 ( 0.005258105385878707357, 0.005948373736081385803 ),
 .UNSPECIFIED. ) ;
#7541 = FACE_OUTER_BOUND ( 'NONE', #4320, .T. ) ;
#7542 = DIRECTION ( 'NONE',  ( 1.000000000000000000, 0.000000000000000000, -0.000000000000000000 ) ) ;
#7543 = FACE_OUTER_BOUND ( 'NONE', #10850, .T. ) ;
#7544 = AXIS2_PLACEMENT_3D ( 'NONE', #13141, #7235, #6085 ) ;
#7545 = B_SPLINE_CURVE_WITH_KNOTS ( 'NONE', 3,
 ( #5690, #11515, #11657, #12741 ),
 .UNSPECIFIED., .F., .F.,
 ( 4, 4 ),
 ( 0.005342776758202895035, 0.005948405594583416715 ),
 .UNSPECIFIED. ) ;
#7546 = CARTESIAN_POINT ( 'NONE',  ( 2.789999999999999147, -23.48180575137734039, 5.535312321042630934 ) ) ;
#7547 = APPLICATION_CONTEXT ( 'automotive_design' ) ;
#7548 = EDGE_LOOP ( 'NONE', ( #6893, #11644, #10604, #7925 ) ) ;
#7549 = CARTESIAN_POINT ( 'NONE',  ( 2.789999999999999147, 0.000000000000000000, 0.000000000000000000 ) ) ;
#7550 = AXIS2_PLACEMENT_3D ( 'NONE', #3818, #7518, #14516 ) ;
#7551=STYLED_ITEM('',(#15258),#3822);
#7552 = VERTEX_POINT ( 'NONE', #13259 ) ;
#7553 = ORIENTED_EDGE ( 'NONE', *, *, #8532, .F. ) ;
#7554 = ORIENTED_EDGE ( 'NONE', *, *, #130, .F. ) ;
#7555 = CARTESIAN_POINT ( 'NONE',  ( 2.765633920072235075, -12.59161484032896361, -21.30679549418645280 ) ) ;
#7556 = CARTESIAN_POINT ( 'NONE',  ( 0.3363705501000965326, -6.891763197764913862, 4.000000000000000000 ) ) ;
#7557 = VERTEX_POINT ( 'NONE', #8490 ) ;
#7558 = STYLED_ITEM ( 'NONE', ( #3031 ), #14983 ) ;
#7559 = CYLINDRICAL_SURFACE ( 'NONE', #2100, 4.000000000000000000 ) ;
#7560 = ORIENTED_EDGE ( 'NONE', *, *, #11140, .T. ) ;
#7561 = CARTESIAN_POINT ( 'NONE',  ( 1.749999999999998002, -12.52377138324241734, 25.12109765559649688 ) ) ;
#7562 = DIRECTION ( 'NONE',  ( 0.000000000000000000, 0.000000000000000000, 1.000000000000000000 ) ) ;
#7563 = DIRECTION ( 'NONE',  ( 0.000000000000000000, 0.000000000000000000, 1.000000000000000000 ) ) ;
#7564 = CARTESIAN_POINT ( 'NONE',  ( 1.749999999999998002, 27.68468304288259318, 4.633866840649019103 ) ) ;
#7565 = ADVANCED_FACE ( 'NONE', ( #13181 ), #2667, .F. ) ;
#7566 = CARTESIAN_POINT ( 'NONE',  ( 0.1855657168891856057, 12.84444904262024956, 22.53097606932990260 ) ) ;
#7567 = CIRCLE ( 'NONE', #11957, 2.000000000000003109 ) ;
#7568 = VERTEX_POINT ( 'NONE', #13725 ) ;
#7569 = CYLINDRICAL_SURFACE ( 'NONE', #11204, 4.999999999999997335 ) ;
#7570 = ADVANCED_FACE ( 'NONE', ( #4124 ), #1190, .T. ) ;
#7571 = CARTESIAN_POINT ( 'NONE',  ( 2.789999999999999147, 14.59528211760002137, -3.120158876139080828 ) ) ;
#7572 = VERTEX_POINT ( 'NONE', #4431 ) ;
#7573 = VERTEX_POINT ( 'NONE', #3123 ) ;
#7574 = CARTESIAN_POINT ( 'NONE',  ( -16.96657417111497068, -13.60061260430328467, -3.794707603699265519E-15 ) ) ;
#7575 = CLOSED_SHELL ( 'NONE', ( #2722, #7649, #2317, #2833, #3856, #11418, #3633, #9994, #7970, #11632, #11713, #8222, #8160, #6264, #14278, #2707, #10563, #521, #11797, #1666, #7525, #917, #12100, #1195, #3388, #13369, #9708, #5460, #6746, #1291, #2279, #8307, #11449, #7405, #11162, #3557, #15165, #6038, #3184, #12820, #12345, #5051, #10783, #7699, #8140, #6740, #13486, #9428, #9848, #2178, #5133, #13774, #9635, #1870, #10217, #3055, #6228, #4520, #10706, #1467, #7570, #6859, #848, #11156, #8789, #787, #9150, #11409, #10323, #164, #14166, #7311, #11284, #13595, #5187, #10515, #9840, #12859, #3543, #11982, #8878, #4138, #2154, #6428, #4790, #10952, #11066, #5510, #2343, #6291, #1103, #10320, #10580, #12153, #3783, #3949, #13517, #12090, #9913, #3513, #1016, #14420, #13642, #14490, #12476, #11086, #930, #560, #4894, #7499, #345, #811, #6368, #14937, #3851, #10868, #8402, #645, #147, #9773, #5798, #13674, #1511, #2250, #12607, #5905, #306, #11603, #13873, #7310, #13007, #10124, #11731 ) ) ;
#7576 = ADVANCED_FACE ( 'NONE', ( #1890 ), #7083, .T. ) ;
#7577 = FACE_BOUND ( 'NONE', #1551, .T. ) ;
#7578 = DIRECTION ( 'NONE',  ( 0.000000000000000000, 0.000000000000000000, 1.000000000000000000 ) ) ;
#7579 = AXIS2_PLACEMENT_3D ( 'NONE', #3348, #8040, #12717 ) ;
#7580 = AXIS2_PLACEMENT_3D ( 'NONE', #100, #4823, #4907 ) ;
#7581 = ORIENTED_EDGE ( 'NONE', *, *, #9111, .T. ) ;
#7582 = CARTESIAN_POINT ( 'NONE',  ( 0.02436607992776281678, 2.336989772644269436, 24.63872515616083447 ) ) ;
#7583 = CARTESIAN_POINT ( 'NONE',  ( 1.039999999999995595, 4.147968289691676524, -27.76164181293047051 ) ) ;
#7584 = FACE_OUTER_BOUND ( 'NONE', #8572, .T. ) ;
#7585 = EDGE_CURVE ( 'NONE', #12816, #7568, #10992, .T. ) ;
#7586 = ADVANCED_FACE ( 'NONE', ( #5661 ), #1689, .T. ) ;
#7587 = EDGE_LOOP ( 'NONE', ( #7162, #14662 ) ) ;
#7588 = ORIENTED_EDGE ( 'NONE', *, *, #7792, .T. ) ;
#7589 = ORIENTED_EDGE ( 'NONE', *, *, #511, .T. ) ;
#7590 = AXIS2_PLACEMENT_3D ( 'NONE', #1148, #5918, #8070 ) ;
#7591 = AXIS2_PLACEMENT_3D ( 'NONE', #7252, #314, #2555 ) ;
#7592 = CARTESIAN_POINT ( 'NONE',  ( 0.5321745379877909077, -23.74442027961350377, -12.96514671151793507 ) ) ;
#7593 = AXIS2_PLACEMENT_3D ( 'NONE', #14671, #668, #14748 ) ;
#7594 = FACE_OUTER_BOUND ( 'NONE', #13061, .T. ) ;
#7595 = CARTESIAN_POINT ( 'NONE',  ( 0.02436607992776151574, -18.55949924794880346, -16.37294372382878649 ) ) ;
#7596 = CARTESIAN_POINT ( 'NONE',  ( 2.764680872513935128, -5.229914364928447412, 13.68080036884346917 ) ) ;
#7597 = PRODUCT_CONTEXT ( 'NONE', #1833, 'mechanical' ) ;
#7598 = DIRECTION ( 'NONE',  ( 0.000000000000000000, 0.000000000000000000, 1.000000000000000000 ) ) ;
#7599 = FACE_OUTER_BOUND ( 'NONE', #2166, .T. ) ;
#7600 = EDGE_CURVE ( 'NONE', #988, #8601, #10276, .T. ) ;
#7601 = ORIENTED_EDGE ( 'NONE', *, *, #3878, .T. ) ;
#7602 = DIRECTION ( 'NONE',  ( -0.4036950204470279302, 0.9148936170212763619, 0.000000000000000000 ) ) ;
#7603 = CARTESIAN_POINT ( 'NONE',  ( -16.14082873121598993, -7.414910804916202913, -3.800000000000000266 ) ) ;
#7604 = CIRCLE ( 'NONE', #2202, 2.524999999999999467 ) ;
#7605 = CARTESIAN_POINT ( 'NONE',  ( -4.000000000000000888, 2.270693314922320170E-33, 7.799999999999990052 ) ) ;
#7606 = ADVANCED_FACE ( 'NONE', ( #10036 ), #5627, .T. ) ;
#7607 = EDGE_CURVE ( 'NONE', #12819, #10457, #12410, .T. ) ;
#7608 = ORIENTED_EDGE ( 'NONE', *, *, #8713, .F. ) ;
#7609 = CARTESIAN_POINT ( 'NONE',  ( 2.246812931352481169, -11.42270873787301610, 12.54666350726119717 ) ) ;
#7610 = DIRECTION ( 'NONE',  ( 0.000000000000000000, 0.000000000000000000, 1.000000000000000000 ) ) ;
#7611 = EDGE_LOOP ( 'NONE', ( #11819, #10038, #3925, #10587, #14591, #4572, #10111, #461 ) ) ;
#7612 = ORIENTED_EDGE ( 'NONE', *, *, #7437, .F. ) ;
#7613 = LINE ( 'NONE', #8605, #157 ) ;
#7614 = EDGE_CURVE ( 'NONE', #1974, #4433, #732, .T. ) ;
#7615 = CARTESIAN_POINT ( 'NONE',  ( 2.030753603471112889, -12.98165646470063983, -24.32906614999630790 ) ) ;
#7616 = CARTESIAN_POINT ( 'NONE',  ( 2.789999999999999147, 7.772527002114753003, -23.17675759782032685 ) ) ;
#7617 = CIRCLE ( 'NONE', #7378, 5.000000000000000888 ) ;
#7618 = DIRECTION ( 'NONE',  ( 1.000000000000000000, -0.000000000000000000, -0.000000000000000000 ) ) ;
#7619 = CARTESIAN_POINT ( 'NONE',  ( 2.764680872513208154, 9.232963481057765875, 11.36963888406690870 ) ) ;
#7620 = ORIENTED_EDGE ( 'NONE', *, *, #3365, .T. ) ;
#7621 = CARTESIAN_POINT ( 'NONE',  ( 1.566204647097437341, -6.822536405429464601, 0.000000000000000000 ) ) ;
#7622 = CARTESIAN_POINT ( 'NONE',  ( 88.46153288930041469, 16.46030115554384565, 4.000000000000000000 ) ) ;
#7623 = FILL_AREA_STYLE ('',( #8842 ) ) ;
#7624 = EDGE_LOOP ( 'NONE', ( #737, #2834 ) ) ;
#7625 = ORIENTED_EDGE ( 'NONE', *, *, #10486, .T. ) ;
#7626 = EDGE_LOOP ( 'NONE', ( #11631, #3180, #11821, #7342 ) ) ;
#7627 = CARTESIAN_POINT ( 'NONE',  ( 2.782650468023970536, -14.24968354755769973, 2.217353748341881481 ) ) ;
#7628 = LINE ( 'NONE', #5336, #6262 ) ;
#7629 = EDGE_CURVE ( 'NONE', #9391, #14971, #3812, .T. ) ;
#7630 = PRODUCT_DEFINITION_CONTEXT ( 'detailed design', #13013, 'design' ) ;
#7631 = DIRECTION ( 'NONE',  ( -1.000000000000000000, -0.000000000000000000, -0.000000000000000000 ) ) ;
#7632 = CARTESIAN_POINT ( 'NONE',  ( 1.000000000000000000, -4.808326913195983821, -0.8000000000000000444 ) ) ;
#7633 = ORIENTED_EDGE ( 'NONE', *, *, #2998, .T. ) ;
#7634 = DIRECTION ( 'NONE',  ( 1.000000000000000000, -0.000000000000000000, -0.000000000000000000 ) ) ;
#7635 = LINE ( 'NONE', #628, #10997 ) ;
#7636 = CYLINDRICAL_SURFACE ( 'NONE', #8436, 8.400000000000000355 ) ;
#7637 = CARTESIAN_POINT ( 'NONE',  ( 2.765633920072236851, 24.15498966839963302, 5.391175441198700291 ) ) ;
#7638 = EDGE_CURVE ( 'NONE', #8287, #6623, #12404, .T. ) ;
#7639 = B_SPLINE_CURVE_WITH_KNOTS ( 'NONE', 3,
 ( #15173, #4646, #4485, #3324 ),
 .UNSPECIFIED., .F., .F.,
 ( 4, 4 ),
 ( 0.005258139959819225183, 0.005948405594583413246 ),
 .UNSPECIFIED. ) ;
#7640 = LINE ( 'NONE', #6477, #5101 ) ;
#7641 = ORIENTED_EDGE ( 'NONE', *, *, #7871, .F. ) ;
#7642 = CARTESIAN_POINT ( 'NONE',  ( 1.749999999999999778, -17.39253030560838198, -4.458161950358684678 ) ) ;
#7643 = CARTESIAN_POINT ( 'NONE',  ( 2.697960371751379594, -11.73065272960056049, -9.756102650610364080 ) ) ;
#7644 = ORIENTED_EDGE ( 'NONE', *, *, #8412, .T. ) ;
#7645 = ORIENTED_EDGE ( 'NONE', *, *, #3259, .F. ) ;
#7646 = DIRECTION ( 'NONE',  ( 0.000000000000000000, 0.000000000000000000, -1.000000000000000000 ) ) ;
#7647 = CARTESIAN_POINT ( 'NONE',  ( 0.000000000000000000, 0.000000000000000000, 10.00000000000000000 ) ) ;
#7648 = FACE_OUTER_BOUND ( 'NONE', #7207, .T. ) ;
#7649 = ADVANCED_FACE ( 'NONE', ( #7809 ), #12630, .T. ) ;
#7650 = CARTESIAN_POINT ( 'NONE',  ( 2.764680872515352217, 14.46287784598617243, 2.311161484776605324 ) ) ;
#7651 = EDGE_CURVE ( 'NONE', #13868, #7028, #4347, .T. ) ;
#7652 = EDGE_LOOP ( 'NONE', ( #3443, #14878, #5659, #6014 ) ) ;
#7653 = DIRECTION ( 'NONE',  ( -5.480158469902919838E-17, -1.051478716308701618E-16, -1.000000000000000000 ) ) ;
#7654 = CARTESIAN_POINT ( 'NONE',  ( -7.816002369513581784E-14, 15.96555658743763217, 18.34439787333512939 ) ) ;
#7655 = ORIENTED_EDGE ( 'NONE', *, *, #2240, .F. ) ;
#7656 = ORIENTED_EDGE ( 'NONE', *, *, #7607, .F. ) ;
#7657 = EDGE_LOOP ( 'NONE', ( #12164, #13793, #1438, #6995, #11289, #9610 ) ) ;
#7658 = CIRCLE ( 'NONE', #6186, 28.06981291497571007 ) ;
#7659 = EDGE_LOOP ( 'NONE', ( #12586, #10041, #13264, #6772 ) ) ;
#7660 = CARTESIAN_POINT ( 'NONE',  ( 1.039999999999996705, -19.67366047555515252, -20.02152543075367319 ) ) ;
#7661 = CARTESIAN_POINT ( 'NONE',  ( 1.039999999999999147, 12.52377138324259676, -25.12109765559640095 ) ) ;
#7662 = DIRECTION ( 'NONE',  ( 1.000000000000000000, 0.000000000000000000, 0.000000000000000000 ) ) ;
#7663 = FACE_OUTER_BOUND ( 'NONE', #5710, .T. ) ;
#7664 =( NAMED_UNIT ( * ) SI_UNIT ( $, .STERADIAN. ) SOLID_ANGLE_UNIT ( ) );
#7665 = CARTESIAN_POINT ( 'NONE',  ( 0.9041604711286022056, -12.27244837507622499, 12.77651625388895162 ) ) ;
#7666 = DIRECTION ( 'NONE',  ( 1.000000000000000000, 0.000000000000000000, -0.000000000000000000 ) ) ;
#7667 = CARTESIAN_POINT ( 'NONE',  ( 2.765633920072235519, -9.836394144775869819, 22.71065055754449347 ) ) ;
#7668 = ORIENTED_EDGE ( 'NONE', *, *, #12045, .F. ) ;
#7670 = CIRCLE ( 'NONE', #1039, 2.524999999999995914 ) ;
#7669 = CARTESIAN_POINT ( 'NONE',  ( 75.20570977803312473, 12.97982004111160315, 6.000000000000000000 ) ) ;
#7671 = CARTESIAN_POINT ( 'NONE',  ( 1.749999999999998002, 27.68468304288265358, -4.633866840648635410 ) ) ;
#7672 = FACE_OUTER_BOUND ( 'NONE', #9026, .T. ) ;
#7673 = ORIENTED_EDGE ( 'NONE', *, *, #14370, .T. ) ;
#7674 = EDGE_CURVE ( 'NONE', #1813, #7692, #10447, .T. ) ;
#7675 = B_SPLINE_CURVE_WITH_KNOTS ( 'NONE', 3,
 ( #8371, #3687, #13050, #14301, #2617, #10835, #5012, #8529 ),
 .UNSPECIFIED., .F., .F.,
 ( 4, 2, 2, 4 ),
 ( 2.154797737796103340E-07, 0.001895231411415141797, 0.002842739377235821516, 0.003790247343056500802 ),
 .UNSPECIFIED. ) ;
#7676 = CARTESIAN_POINT ( 'NONE',  ( 2.765633920072234631, 5.391175441198615914, 24.15498966839965078 ) ) ;
#7677 = CARTESIAN_POINT ( 'NONE',  ( 2.789999999999999147, 24.44424927289184879, 0.2301004812061933913 ) ) ;
#7678 = EDGE_LOOP ( 'NONE', ( #14908, #11756, #4922, #286 ) ) ;
#7679 = ORIENTED_EDGE ( 'NONE', *, *, #3088, .F. ) ;
#7680 = DIRECTION ( 'NONE',  ( 1.000000000000000000, 0.000000000000000000, 0.000000000000000000 ) ) ;
#7681 = VECTOR ( 'NONE', #12547, 1000.000000000000000 ) ;
#7682 = CARTESIAN_POINT ( 'NONE',  ( 0.000000000000000000, 1.991882183130641248, -24.04302995059964942 ) ) ;
#7683 = CYLINDRICAL_SURFACE ( 'NONE', #10654, 13.19999999999999929 ) ;
#7684 = CARTESIAN_POINT ( 'NONE',  ( 2.789999999999999147, 0.000000000000000000, 0.000000000000000000 ) ) ;
#7685 = ADVANCED_FACE ( 'NONE', ( #11399 ), #12330, .T. ) ;
#7686 = EDGE_CURVE ( 'NONE', #1104, #852, #5503, .T. ) ;
#7687 = DIRECTION ( 'NONE',  ( 0.000000000000000000, 0.000000000000000000, -1.000000000000000000 ) ) ;
#7688 = CARTESIAN_POINT ( 'NONE',  ( 2.171938186095908829, 23.93436800624300886, 12.96259772325185544 ) ) ;
#7689 = ORIENTED_EDGE ( 'NONE', *, *, #13679, .T. ) ;
#7690 = CARTESIAN_POINT ( 'NONE',  ( 0.000000000000000000, -22.25075486061745167, 9.324097380959385006 ) ) ;
#7691 = DIRECTION ( 'NONE',  ( -1.000000000000000000, 0.000000000000000000, 0.000000000000000000 ) ) ;
#7692 = VERTEX_POINT ( 'NONE', #7174 ) ;
#7693 = SHAPE_REPRESENTATION_RELATIONSHIP ( 'NONE' , 'NONE' ,  #13067, #8180 ) ;
#7694 = ORIENTED_EDGE ( 'NONE', *, *, #4779, .F. ) ;
#7695 = ORIENTED_EDGE ( 'NONE', *, *, #6055, .T. ) ;
#7696 = ORIENTED_EDGE ( 'NONE', *, *, #6198, .T. ) ;
#7697 = EDGE_CURVE ( 'NONE', #5464, #2195, #1033, .T. ) ;
#7698 = CARTESIAN_POINT ( 'NONE',  ( 2.790000000000076863, -12.51293083811783191, -20.85287692521943015 ) ) ;
#7699 = ADVANCED_FACE ( 'NONE', ( #8173 ), #12846, .T. ) ;
#7700 = CARTESIAN_POINT ( 'NONE',  ( 2.765633920072234631, 16.37294372382885044, -18.55949924794875017 ) ) ;
#7701 = EDGE_CURVE ( 'NONE', #2991, #8100, #15031, .T. ) ;
#7702 = CARTESIAN_POINT ( 'NONE',  ( 18.71314632718394222, -23.25585687728512241, 2.000000000000000000 ) ) ;
#7703 = DIRECTION ( 'NONE',  ( -1.000000000000000000, 0.000000000000000000, 0.000000000000000000 ) ) ;
#7704 = ORIENTED_EDGE ( 'NONE', *, *, #574, .T. ) ;
#7705 = CARTESIAN_POINT ( 'NONE',  ( 2.601776144743012775, -10.68696068830424473, 23.64332819722378076 ) ) ;
#7706 = LINE ( 'NONE', #6473, #4127 ) ;
#7707 = EDGE_CURVE ( 'NONE', #11802, #2246, #6237, .T. ) ;
#7708 = DIRECTION ( 'NONE',  ( 1.000000000000000000, 0.000000000000000000, 0.000000000000000000 ) ) ;
#7709 = CYLINDRICAL_SURFACE ( 'NONE', #10365, 4.000000000000000888 ) ;
#7710 = AXIS2_PLACEMENT_3D ( 'NONE', #11242, #8782, #6639 ) ;
#7711 = CIRCLE ( 'NONE', #3776, 2.999999999999975131 ) ;
#7712 = ORIENTED_EDGE ( 'NONE', *, *, #2776, .T. ) ;
#7713 = CARTESIAN_POINT ( 'NONE',  ( 0.9041604898882311669, 17.01651022436369942, -4.928563447326111735 ) ) ;
#7714 = CARTESIAN_POINT ( 'NONE',  ( 2.740003299868483566, -11.55877992729658565, -9.490919315500255138 ) ) ;
#7715 = CIRCLE ( 'NONE', #12610, 17.95481323787947403 ) ;
#7716 = VERTEX_POINT ( 'NONE', #11843 ) ;
#7717 = ORIENTED_EDGE ( 'NONE', *, *, #14272, .F. ) ;
#7718 = DIRECTION ( 'NONE',  ( 1.000000000000000000, 0.000000000000000000, 0.000000000000000000 ) ) ;
#7719 = CARTESIAN_POINT ( 'NONE',  ( 1.039999999999996483, -19.67366047555544384, 20.02152543075338897 ) ) ;
#7720 = AXIS2_PLACEMENT_3D ( 'NONE', #4781, #3688, #3614 ) ;
#7721 = ORIENTED_EDGE ( 'NONE', *, *, #4041, .F. ) ;
#7722=STYLED_ITEM('',(#15265),#8383);
#7723 = LINE ( 'NONE', #12408, #12932 ) ;
#7724 = VECTOR ( 'NONE', #10896, 1000.000000000000000 ) ;
#7725 = VERTEX_POINT ( 'NONE', #1108 ) ;
#7726 = CARTESIAN_POINT ( 'NONE',  ( 2.257825491203657275, 11.58891744060141882, -24.44564404695831783 ) ) ;
#7727 = DIRECTION ( 'NONE',  ( -1.000000000000000000, 0.000000000000000000, 0.000000000000000000 ) ) ;
#7728 = ORIENTED_EDGE ( 'NONE', *, *, #5653, .F. ) ;
#7729 = LINE ( 'NONE', #8872, #160 ) ;
#7730 = EDGE_LOOP ( 'NONE', ( #12067, #14757, #3290, #3883 ) ) ;
#7731 = VERTEX_POINT ( 'NONE', #13000 ) ;
#7732 = AXIS2_PLACEMENT_3D ( 'NONE', #6281, #2821, #2975 ) ;
#7733 = TOROIDAL_SURFACE ( 'NONE', #1102, 24.12539914357697413, 8.000000000000000000 ) ;
#7734 = AXIS2_PLACEMENT_3D ( 'NONE', #13613, #9852, #5254 ) ;
#7735 = ORIENTED_EDGE ( 'NONE', *, *, #12147, .F. ) ;
#7736 = CARTESIAN_POINT ( 'NONE',  ( -10.40394475573011945, -10.79473832354794460, -5.000000000000000000 ) ) ;
#7737 = EDGE_CURVE ( 'NONE', #10625, #4617, #10564, .T. ) ;
#7738 = LINE ( 'NONE', #11493, #2638 ) ;
#7739 = DIRECTION ( 'NONE',  ( -1.000000000000000000, -0.000000000000000000, -0.000000000000000000 ) ) ;
#7740 = CARTESIAN_POINT ( 'NONE',  ( 88.84370878116858705, 10.64188714589527507, 2.999999999999999112 ) ) ;
#7741 = DIRECTION ( 'NONE',  ( 0.000000000000000000, 0.000000000000000000, -1.000000000000000000 ) ) ;
#7742 = DIRECTION ( 'NONE',  ( -1.000000000000000000, -0.000000000000000000, -0.000000000000000000 ) ) ;
#7743 = AXIS2_PLACEMENT_3D ( 'NONE', #9174, #5722, #10394 ) ;
#7744 = ORIENTED_EDGE ( 'NONE', *, *, #14074, .F. ) ;
#7745 = DIRECTION ( 'NONE',  ( 1.000000000000000000, 0.000000000000000000, 0.000000000000000000 ) ) ;
#7746 = CIRCLE ( 'NONE', #9705, 4.000000000000000000 ) ;
#7747 = DIRECTION ( 'NONE',  ( 0.000000000000000000, 0.000000000000000000, 1.000000000000000000 ) ) ;
#7748 = AXIS2_PLACEMENT_3D ( 'NONE', #7947, #4271, #6720 ) ;
#7749 = FACE_OUTER_BOUND ( 'NONE', #14904, .T. ) ;
#7750 = ORIENTED_EDGE ( 'NONE', *, *, #3195, .F. ) ;
#7751 = DIRECTION ( 'NONE',  ( 0.000000000000000000, 0.000000000000000000, 1.000000000000000000 ) ) ;
#7752 = CARTESIAN_POINT ( 'NONE',  ( 0.000000000000000000, -15.74360496233370021, -18.28042085475294698 ) ) ;
#7753 = ORIENTED_EDGE ( 'NONE', *, *, #3036, .T. ) ;
#7754 = ORIENTED_EDGE ( 'NONE', *, *, #804, .F. ) ;
#7755 = CYLINDRICAL_SURFACE ( 'NONE', #4360, 2.524999999999995914 ) ;
#7756 = CIRCLE ( 'NONE', #3100, 28.06981291497571007 ) ;
#7757 = CARTESIAN_POINT ( 'NONE',  ( 65.21556745095632834, 33.50594455047664866, -2.000000000000000000 ) ) ;
#7758 = EDGE_CURVE ( 'NONE', #2957, #4474, #9337, .T. ) ;
#7759 = CARTESIAN_POINT ( 'NONE',  ( 58.14665764790533586, -0.9105996816177498454, 3.000000000000000000 ) ) ;
#7760 = DIRECTION ( 'NONE',  ( 1.445602896647338917E-16, -1.000000000000000000, 0.000000000000000000 ) ) ;
#7761 = CARTESIAN_POINT ( 'NONE',  ( 2.789999999999999147, 7.909232158575156824, -24.34211360614291664 ) ) ;
#7762 = EDGE_CURVE ( 'NONE', #2008, #12014, #591, .T. ) ;
#7763 = CARTESIAN_POINT ( 'NONE',  ( -14.40394475573011945, -10.79473832354794460, -3.000000000000000000 ) ) ;
#7764 = CARTESIAN_POINT ( 'NONE',  ( 2.351340098004231383, 23.41653927703715965, 12.93238701107315514 ) ) ;
#7765 = ORIENTED_EDGE ( 'NONE', *, *, #11989, .F. ) ;
#7766 = AXIS2_PLACEMENT_3D ( 'NONE', #3601, #9438, #3456 ) ;
#7767 = CARTESIAN_POINT ( 'NONE',  ( -10.40394475573011945, -10.79473832354794460, -3.800000000000000266 ) ) ;
#7768 = CIRCLE ( 'NONE', #3109, 2.999999999999975131 ) ;
#7769 = DIRECTION ( 'NONE',  ( -0.000000000000000000, -0.000000000000000000, 1.000000000000000000 ) ) ;
#7770 = ORIENTED_EDGE ( 'NONE', *, *, #10029, .F. ) ;
#7771 = PRODUCT_DEFINITION ( 'UNKNOWN', '', #2089, #13466 ) ;
#7772 = EDGE_CURVE ( 'NONE', #8240, #3993, #12708, .T. ) ;
#7773 = ADVANCED_FACE ( 'NONE', ( #15105 ), #2336, .T. ) ;
#7774 = ORIENTED_EDGE ( 'NONE', *, *, #15010, .T. ) ;
#7775 = ORIENTED_EDGE ( 'NONE', *, *, #8037, .F. ) ;
#7776 = ORIENTED_EDGE ( 'NONE', *, *, #3539, .F. ) ;
#7777 = DIRECTION ( 'NONE',  ( -1.000000000000000000, -0.000000000000000000, -0.000000000000000000 ) ) ;
#7778 = DIRECTION ( 'NONE',  ( -2.081668171172168513E-16, 1.000000000000000000, 0.000000000000000000 ) ) ;
#7779 = CIRCLE ( 'NONE', #1150, 2.524999999999995914 ) ;
#7780 = CIRCLE ( 'NONE', #8258, 2.524999999999995914 ) ;
#7781=STYLED_ITEM('',(#15265),#13393);
#7782 = DIRECTION ( 'NONE',  ( 0.000000000000000000, 0.000000000000000000, 1.000000000000000000 ) ) ;
#7783 = CIRCLE ( 'NONE', #9485, 4.000000000000000000 ) ;
#7784 = CARTESIAN_POINT ( 'NONE',  ( 1.039999999999996261, 4.458161950358501713, 17.39253030560843172 ) ) ;
#7785 = ORIENTED_EDGE ( 'NONE', *, *, #2708, .F. ) ;
#7786 = FACE_BOUND ( 'NONE', #1233, .T. ) ;
#7787 = CARTESIAN_POINT ( 'NONE',  ( 2.789999999999999147, 1.948757464274172513, 13.87420763704361804 ) ) ;
#7788 = EDGE_CURVE ( 'NONE', #12063, #2289, #5696, .T. ) ;
#7789 = CARTESIAN_POINT ( 'NONE',  ( -3.751931928061364552, 0.6025004624012588739, 6.999999999999989342 ) ) ;
#7790 = CIRCLE ( 'NONE', #10246, 24.12539914357697413 ) ;
#7791 = CARTESIAN_POINT ( 'NONE',  ( 0.02436607992775934733, -21.30679549418640306, 12.59161484032904887 ) ) ;
#7792 = EDGE_CURVE ( 'NONE', #9957, #7850, #10828, .T. ) ;
#7793 = CIRCLE ( 'NONE', #10490, 24.12539914357697768 ) ;
#7794 = ORIENTED_EDGE ( 'NONE', *, *, #5278, .T. ) ;
#7795 = VECTOR ( 'NONE', #2451, 1000.000000000000000 ) ;
#7796 = DIRECTION ( 'NONE',  ( -0.000000000000000000, -0.000000000000000000, 1.000000000000000000 ) ) ;
#7797 = CARTESIAN_POINT ( 'NONE',  ( 0.1085714285714285687, -3.798448662927795372, -0.8000000000000000444 ) ) ;
#7798 = COLOUR_RGB ( '',1.000000000000000000, 0.9490196078431372140, 0.9098039215686274384 ) ;
#7799 = ORIENTED_EDGE ( 'NONE', *, *, #2526, .F. ) ;
#7800 = ORIENTED_EDGE ( 'NONE', *, *, #13476, .T. ) ;
#7801 = CARTESIAN_POINT ( 'NONE',  ( 2.789999999999999147, -13.40591150984221080, -7.739906618939849103 ) ) ;
#7802 = EDGE_CURVE ( 'NONE', #4654, #14563, #5885, .T. ) ;
#7803 = SURFACE_STYLE_USAGE ( .BOTH. , #2102 ) ;
#7804 = DIRECTION ( 'NONE',  ( 1.000000000000000000, 0.000000000000000000, -0.000000000000000000 ) ) ;
#7805 = ORIENTED_EDGE ( 'NONE', *, *, #9002, .F. ) ;
#7806 = AXIS2_PLACEMENT_3D ( 'NONE', #5638, #10461, #3465 ) ;
#7807 = CARTESIAN_POINT ( 'NONE',  ( 2.764680872515352661, -9.232963481057844035, 11.36963888406684298 ) ) ;
#7808 = ORIENTED_EDGE ( 'NONE', *, *, #3186, .F. ) ;
#7809 = FACE_OUTER_BOUND ( 'NONE', #10570, .T. ) ;
#7810 = DIRECTION ( 'NONE',  ( -1.000000000000000000, 0.000000000000000000, 0.000000000000000000 ) ) ;
#7811 = CIRCLE ( 'NONE', #12468, 4.000000000000000000 ) ;
#7812 = AXIS2_PLACEMENT_3D ( 'NONE', #14402, #14246, #3870 ) ;
#7813 = ORIENTED_EDGE ( 'NONE', *, *, #7674, .F. ) ;
#7814 = FILL_AREA_STYLE ('',( #3342 ) ) ;
#7815 = DIRECTION ( 'NONE',  ( 1.000000000000000000, 0.000000000000000000, 0.000000000000000000 ) ) ;
#7816 = ORIENTED_EDGE ( 'NONE', *, *, #7033, .T. ) ;
#7817 = B_SPLINE_CURVE_WITH_KNOTS ( 'NONE', 3,
 ( #11077, #11145, #620, #12143 ),
 .UNSPECIFIED., .F., .F.,
 ( 4, 4 ),
 ( 2.451234579287542699E-07, 0.0006917187676826498915 ),
 .UNSPECIFIED. ) ;
#7818 = VERTEX_POINT ( 'NONE', #13947 ) ;
#7819 = AXIS2_PLACEMENT_3D ( 'NONE', #12590, #5760, #5540 ) ;
#7820 = FACE_OUTER_BOUND ( 'NONE', #2806, .T. ) ;
#7821 = CARTESIAN_POINT ( 'NONE',  ( 101.6227766016837819, 5.204170427930421283E-15, 7.000000000000006217 ) ) ;
#7822 = CARTESIAN_POINT ( 'NONE',  ( 101.6227766016837819, -9.999999999999994671, -131.1575142076926852 ) ) ;
#7823 = APPLICATION_PROTOCOL_DEFINITION ( 'draft international standard', 'automotive_design', 1998, #4987 ) ;
#7824 = CIRCLE ( 'NONE', #9785, 24.12539914357697768 ) ;
#7825 = DIRECTION ( 'NONE',  ( -1.000000000000000000, -0.000000000000000000, -0.000000000000000000 ) ) ;
#7826 = DIRECTION ( 'NONE',  ( 1.576560579138138762E-17, -1.359337748750801762E-17, 1.000000000000000000 ) ) ;
#7827 = EDGE_LOOP ( 'NONE', ( #4192, #13937, #14547, #2184, #8460, #5410 ) ) ;
#7828 = CARTESIAN_POINT ( 'NONE',  ( 2.508169649284525793, 3.072260951847751720, -15.84037596932104464 ) ) ;
#7829 = CARTESIAN_POINT ( 'NONE',  ( 98.63205416320636232, -2.094184955359725375, -2.000000000000000888 ) ) ;
#7830 = LINE ( 'NONE', #14901, #3599 ) ;
#7831 = ORIENTED_EDGE ( 'NONE', *, *, #2531, .T. ) ;
#7832 = CIRCLE ( 'NONE', #4647, 14.01039946648073986 ) ;
#7833 = AXIS2_PLACEMENT_3D ( 'NONE', #8867, #4345, #13562 ) ;
#7834 = VECTOR ( 'NONE', #11496, 1000.000000000000000 ) ;
#7835 = EDGE_CURVE ( 'NONE', #10776, #1519, #10488, .T. ) ;
#7836 = CARTESIAN_POINT ( 'NONE',  ( 2.789999999999999147, -11.36963888406680923, -9.232963481057881339 ) ) ;
#7837 = DIRECTION ( 'NONE',  ( 1.000000000000000000, 1.445602896647338917E-16, -0.000000000000000000 ) ) ;
#7838 = ORIENTED_EDGE ( 'NONE', *, *, #331, .F. ) ;
#7839 = VERTEX_POINT ( 'NONE', #1255 ) ;
#7840 = DIRECTION ( 'NONE',  ( 1.000000000000000000, 0.000000000000000000, 0.000000000000000000 ) ) ;
#7841 = CARTESIAN_POINT ( 'NONE',  ( 2.764680872513937349, -13.68080036884344963, -5.229914364928496262 ) ) ;
#7842 = ORIENTED_EDGE ( 'NONE', *, *, #13746, .T. ) ;
#7843 = CARTESIAN_POINT ( 'NONE',  ( 4.747884751462026820, -5.143694235355983579, -0.8000000000000000444 ) ) ;
#7844 = CARTESIAN_POINT ( 'NONE',  ( 2.789999999999999147, -9.232963481057844035, 11.36963888406684298 ) ) ;
#7845 = CARTESIAN_POINT ( 'NONE',  ( 2.789999999999999147, -5.535312321042557215, -23.48180575137735815 ) ) ;
#7846 = DIRECTION ( 'NONE',  ( 1.000000000000000000, 0.000000000000000000, 0.000000000000000000 ) ) ;
#7847 = CARTESIAN_POINT ( 'NONE',  ( 88.84370878116858705, 10.64188714589527507, 2.999999999999999112 ) ) ;
#7848 = VECTOR ( 'NONE', #8304, 1000.000000000000000 ) ;
#7849 = EDGE_CURVE ( 'NONE', #7151, #12400, #81, .T. ) ;
#7850 = VERTEX_POINT ( 'NONE', #14172 ) ;
#7851 = DIRECTION ( 'NONE',  ( 0.000000000000000000, 0.000000000000000000, 1.000000000000000000 ) ) ;
#7852 = DIRECTION ( 'NONE',  ( -0.000000000000000000, -0.000000000000000000, 1.000000000000000000 ) ) ;
#7853 = EDGE_CURVE ( 'NONE', #3507, #3292, #2723, .T. ) ;
#7854 = VERTEX_POINT ( 'NONE', #396 ) ;
#7855 = FILL_AREA_STYLE_COLOUR ( '', #8746 ) ;
#7856 = EDGE_CURVE ( 'NONE', #12188, #12123, #5118, .T. ) ;
#7857 = EDGE_LOOP ( 'NONE', ( #9985, #2165, #7886, #10347 ) ) ;
#7858 = VERTEX_POINT ( 'NONE', #2867 ) ;
#7859 = VERTEX_POINT ( 'NONE', #9792 ) ;
#7860 = TOROIDAL_SURFACE ( 'NONE', #11528, 14.01039946648073986, 8.000000000000000000 ) ;
#7861 = CARTESIAN_POINT ( 'NONE',  ( 1.885839528871396054, -12.77651625388907775, 12.27244837507608466 ) ) ;
#7862 = LINE ( 'NONE', #12538, #13376 ) ;
#7863 = CARTESIAN_POINT ( 'NONE',  ( 2.789999999999999147, -3.120158876139132342, 14.59528211760001071 ) ) ;
#7864 = EDGE_CURVE ( 'NONE', #3935, #2051, #14842, .T. ) ;
#7865 = ORIENTED_EDGE ( 'NONE', *, *, #6521, .T. ) ;
#7866 = DIRECTION ( 'NONE',  ( 0.000000000000000000, 0.000000000000000000, 1.000000000000000000 ) ) ;
#7867 = FACE_OUTER_BOUND ( 'NONE', #6587, .T. ) ;
#7868 = AXIS2_PLACEMENT_3D ( 'NONE', #1204, #13965, #3431 ) ;
#7869 = CARTESIAN_POINT ( 'NONE',  ( -4.000000000000000888, 2.270693314922320170E-33, 6.999999999999989342 ) ) ;
#7870 = CARTESIAN_POINT ( 'NONE',  ( 0.5321745326902584949, 3.467596033028283564, 26.83036154824995023 ) ) ;
#7871 = EDGE_CURVE ( 'NONE', #11410, #2490, #2788, .T. ) ;
#7872 = VERTEX_POINT ( 'NONE', #6328 ) ;
#7873 = FACE_OUTER_BOUND ( 'NONE', #5982, .T. ) ;
#7874 = CARTESIAN_POINT ( 'NONE',  ( 1.749999999999998002, -4.147968289691086774, -27.76164181293056288 ) ) ;
#7875 = ORIENTED_EDGE ( 'NONE', *, *, #13404, .T. ) ;
#7876 = VERTEX_POINT ( 'NONE', #4956 ) ;
#7877 = EDGE_CURVE ( 'NONE', #11474, #8331, #11013, .T. ) ;
#7878 = CYLINDRICAL_SURFACE ( 'NONE', #9219, 4.999999999999997335 ) ;
#7879 = EDGE_CURVE ( 'NONE', #6222, #6770, #11626, .T. ) ;
#7880 = EDGE_CURVE ( 'NONE', #12279, #11000, #1490, .T. ) ;
#7881 = ORIENTED_EDGE ( 'NONE', *, *, #14598, .T. ) ;
#7882 = PLANE ( 'NONE',  #7833 ) ;
#7883 = VERTEX_POINT ( 'NONE', #14247 ) ;
#7884 = DIRECTION ( 'NONE',  ( 0.000000000000000000, 1.000000000000000000, -1.084202172485504187E-16 ) ) ;
#7885 = CYLINDRICAL_SURFACE ( 'NONE', #13557, 4.000000000000000000 ) ;
#7886 = ORIENTED_EDGE ( 'NONE', *, *, #4383, .T. ) ;
#7887 = DIRECTION ( 'NONE',  ( 1.000000000000000000, 0.000000000000000000, 0.000000000000000000 ) ) ;
#7888 = ORIENTED_EDGE ( 'NONE', *, *, #11482, .F. ) ;
#7889 = ORIENTED_EDGE ( 'NONE', *, *, #8825, .F. ) ;
#7890 = VERTEX_POINT ( 'NONE', #14403 ) ;
#7891 = SHAPE_REPRESENTATION ( 'circlip for shafts normal_din_Circlip DIN 471 - 8 x 0.8', ( #1376 ), #3356 ) ;
#7892 = EDGE_CURVE ( 'NONE', #13731, #2441, #13849, .T. ) ;
#7893 = DIRECTION ( 'NONE',  ( -1.000000000000000000, 0.000000000000000000, 0.000000000000000000 ) ) ;
#7894 = CARTESIAN_POINT ( 'NONE',  ( -16.96657417111497068, -13.60061260430328467, -3.794707603699265519E-15 ) ) ;
#7895 = EDGE_CURVE ( 'NONE', #7177, #1861, #478, .T. ) ;
#7896 = CARTESIAN_POINT ( 'NONE',  ( 1.749999999999998002, -12.52377138324206030, -25.12109765559667096 ) ) ;
#7897 = CARTESIAN_POINT ( 'NONE',  ( 55.83172393217232354, 8.817765129169439220, 4.000000000000000000 ) ) ;
#7898 = DIRECTION ( 'NONE',  ( 0.000000000000000000, 0.5877852522924629231, 0.8090169943749548898 ) ) ;
#7899 = EDGE_CURVE ( 'NONE', #1420, #9357, #4038, .T. ) ;
#7900 = CYLINDRICAL_SURFACE ( 'NONE', #11295, 4.999999999999997335 ) ;
#7901 = EDGE_LOOP ( 'NONE', ( #9151, #8082, #14292, #9298 ) ) ;
#7902 = DIRECTION ( 'NONE',  ( -1.000000000000000000, 0.000000000000000000, -0.000000000000000000 ) ) ;
#7903 = CARTESIAN_POINT ( 'NONE',  ( 1.394999999999999574, -20.02152543075359858, 19.67366047555523778 ) ) ;
#7904 = DIRECTION ( 'NONE',  ( 0.000000000000000000, 0.000000000000000000, 1.000000000000000000 ) ) ;
#7905 = EDGE_CURVE ( 'NONE', #7872, #5284, #7413, .T. ) ;
#7906 = ORIENTED_EDGE ( 'NONE', *, *, #6296, .F. ) ;
#7907 = LINE ( 'NONE', #12583, #8005 ) ;
#7908 = CARTESIAN_POINT ( 'NONE',  ( -3.510166481118844661, -1.455586230640303347, -7.000000000000007994 ) ) ;
#7909 = ORIENTED_EDGE ( 'NONE', *, *, #7707, .T. ) ;
#7910 = ORIENTED_EDGE ( 'NONE', *, *, #2258, .F. ) ;
#7911 = DIRECTION ( 'NONE',  ( 1.000000000000000000, 0.000000000000000000, 0.000000000000000000 ) ) ;
#7912 = CARTESIAN_POINT ( 'NONE',  ( 1.039999999999997593, 0.000000000000000000, 0.000000000000000000 ) ) ;
#7913 = ORIENTED_EDGE ( 'NONE', *, *, #13560, .F. ) ;
#7914 = CARTESIAN_POINT ( 'NONE',  ( 2.789999999999999147, 7.909232158575156824, -21.81711360614291806 ) ) ;
#7915 = LINE ( 'NONE', #7844, #6247 ) ;
#7916 = FILL_AREA_STYLE_COLOUR ( '', #12628 ) ;
#7917 = AXIS2_PLACEMENT_3D ( 'NONE', #5830, #8344, #13020 ) ;
#7918 = CARTESIAN_POINT ( 'NONE',  ( 0.07181523211953112773, 23.19431517146946931, -10.24584646439514657 ) ) ;
#7919 = LINE ( 'NONE', #3163, #4735 ) ;
#7920 = ORIENTED_EDGE ( 'NONE', *, *, #1459, .T. ) ;
#7921 = CARTESIAN_POINT ( 'NONE',  ( 0.02436607992776628623, 24.63872515616082737, -2.336989772644355590 ) ) ;
#7922 = CARTESIAN_POINT ( 'NONE',  ( 2.765633920072236851, 24.15498966839963302, 5.391175441198700291 ) ) ;
#7923 = ORIENTED_EDGE ( 'NONE', *, *, #7880, .F. ) ;
#7924 =( NAMED_UNIT ( * ) PLANE_ANGLE_UNIT ( ) SI_UNIT ( $, .RADIAN. ) );
#7925 = ORIENTED_EDGE ( 'NONE', *, *, #1558, .T. ) ;
#7926 = ORIENTED_EDGE ( 'NONE', *, *, #8626, .T. ) ;
#7927 = ORIENTED_EDGE ( 'NONE', *, *, #14839, .F. ) ;
#7928 = CYLINDRICAL_SURFACE ( 'NONE', #3604, 3.799999999999999378 ) ;
#7929 = CARTESIAN_POINT ( 'NONE',  ( 1.039999999999996927, -25.12109765559644714, -12.52377138324250438 ) ) ;
#7930 = CARTESIAN_POINT ( 'NONE',  ( 0.000000000000000000, 0.000000000000000000, 7.799999999999990052 ) ) ;
#7931 = EDGE_CURVE ( 'NONE', #9391, #5611, #12155, .T. ) ;
#7932 = CARTESIAN_POINT ( 'NONE',  ( 70.16198417812034904, 9.730076655429538590, 7.000000000000000000 ) ) ;
#7933 = VERTEX_POINT ( 'NONE', #9627 ) ;
#7934 = DIRECTION ( 'NONE',  ( -0.9237280213470682178, -0.3830490080632377725, 0.000000000000000000 ) ) ;
#7935 = DIRECTION ( 'NONE',  ( -1.000000000000000000, 0.000000000000000000, 0.000000000000000000 ) ) ;
#7936 = CARTESIAN_POINT ( 'NONE',  ( 0.000000000000000000, 7.739906618939895289, -13.40591150984218416 ) ) ;
#7937 = ORIENTED_EDGE ( 'NONE', *, *, #1964, .F. ) ;
#7938 = CYLINDRICAL_SURFACE ( 'NONE', #6517, 8.400000000000000355 ) ;
#7939 = CARTESIAN_POINT ( 'NONE',  ( 2.789999999999999147, 22.25075486061751207, -9.324097380959219805 ) ) ;
#7940 = ORIENTED_EDGE ( 'NONE', *, *, #11422, .F. ) ;
#7941 = EDGE_LOOP ( 'NONE', ( #13893, #1624, #14371, #12357 ) ) ;
#7942 = DIRECTION ( 'NONE',  ( -1.000000000000000000, -0.000000000000000000, -0.000000000000000000 ) ) ;
#7943 = AXIS2_PLACEMENT_3D ( 'NONE', #8422, #274, #6208 ) ;
#7944 = ORIENTED_EDGE ( 'NONE', *, *, #4665, .F. ) ;
#7945 = EDGE_CURVE ( 'NONE', #7436, #14511, #13837, .T. ) ;
#7946 = DIRECTION ( 'NONE',  ( 0.000000000000000000, 0.000000000000000000, -1.000000000000000000 ) ) ;
#7947 = CARTESIAN_POINT ( 'NONE',  ( 0.000000000000000000, -15.47981323787947794, -1.080949580976661932E-13 ) ) ;
#7948 = DIRECTION ( 'NONE',  ( -5.480158469902919838E-17, -1.051478716308701618E-16, -1.000000000000000000 ) ) ;
#7949 = VERTEX_POINT ( 'NONE', #14559 ) ;
#7950 = CYLINDRICAL_SURFACE ( 'NONE', #4355, 2.524999999999995914 ) ;
#7951 = AXIS2_PLACEMENT_3D ( 'NONE', #6213, #10892, #9747 ) ;
#7952 = EDGE_LOOP ( 'NONE', ( #8424, #8868, #10077, #5608, #13078, #14800 ) ) ;
#7953 = ORIENTED_EDGE ( 'NONE', *, *, #13788, .T. ) ;
#7954 = EDGE_CURVE ( 'NONE', #4522, #11822, #12167, .T. ) ;
#7955 = EDGE_CURVE ( 'NONE', #8927, #2359, #11135, .T. ) ;
#7956 = VERTEX_POINT ( 'NONE', #9709 ) ;
#7957 = PRESENTATION_STYLE_ASSIGNMENT (( #13800 ) ) ;
#7959 = CARTESIAN_POINT ( 'NONE',  ( 0.000000000000000000, 0.000000000000000000, 0.000000000000000000 ) ) ;
#7958 = CIRCLE ( 'NONE', #5281, 2.524999999999999467 ) ;
#7960 = AXIS2_PLACEMENT_3D ( 'NONE', #10837, #4078, #14303 ) ;
#7961 = CARTESIAN_POINT ( 'NONE',  ( 50.00050000000000239, 0.000000000000000000, 0.000000000000000000 ) ) ;
#7962 = VECTOR ( 'NONE', #611, 1000.000000000000000 ) ;
#7963 = CARTESIAN_POINT ( 'NONE',  ( 1.749999999999999778, -4.835383649608602674, 17.29145405592687013 ) ) ;
#7964 = CARTESIAN_POINT ( 'NONE',  ( 2.789999999999999147, -20.70663861606282197, 15.04425356660753188 ) ) ;
#7965 = DIRECTION ( 'NONE',  ( 0.000000000000000000, 1.000000000000000000, 0.000000000000000000 ) ) ;
#7966 = EDGE_LOOP ( 'NONE', ( #2080, #12975, #4369, #4070 ) ) ;
#7967 = CARTESIAN_POINT ( 'NONE',  ( 2.246812880117044386, 3.619024283482299875, -16.57708379306440349 ) ) ;
#7968 = CARTESIAN_POINT ( 'NONE',  ( 98.33955663538051795, 3.898681236723621879, 4.000000000000000000 ) ) ;
#7969 = B_SPLINE_CURVE_WITH_KNOTS ( 'NONE', 3,
 ( #1162, #9680, #59, #2537, #10544, #8300 ),
 .UNSPECIFIED., .F., .F.,
 ( 4, 2, 4 ),
 ( 4.462636678113234028E-07, 0.001879885020955180275, 0.003759323778242549142 ),
 .UNSPECIFIED. ) ;
#7970 = ADVANCED_FACE ( 'NONE', ( #4022 ), #8696, .F. ) ;
#7971 = AXIS2_PLACEMENT_3D ( 'NONE', #1359, #14206, #10527 ) ;
#7972 = CARTESIAN_POINT ( 'NONE',  ( 2.601776121706764311, -17.47009390565504816, 19.18368891937484477 ) ) ;
#7973 = ADVANCED_FACE ( 'NONE', ( #5349 ), #13354, .T. ) ;
#7974 = CIRCLE ( 'NONE', #1587, 3.799999999999998934 ) ;
#7975 = ORIENTED_EDGE ( 'NONE', *, *, #804, .T. ) ;
#7976 = EDGE_CURVE ( 'NONE', #5736, #807, #6973, .T. ) ;
#7977 = DIRECTION ( 'NONE',  ( -1.000000000000000000, 0.000000000000000000, 0.000000000000000000 ) ) ;
#7978 = LINE ( 'NONE', #14989, #14136 ) ;
#7979 = ORIENTED_EDGE ( 'NONE', *, *, #6706, .F. ) ;
#7980 = ORIENTED_EDGE ( 'NONE', *, *, #5458, .F. ) ;
#7981 = DIRECTION ( 'NONE',  ( 0.000000000000000000, 0.000000000000000000, 1.000000000000000000 ) ) ;
#7982 = CARTESIAN_POINT ( 'NONE',  ( -10.00000000000000000, 0.000000000000000000, 0.000000000000000000 ) ) ;
#7983 = VERTEX_POINT ( 'NONE', #7869 ) ;
#7984 = DIRECTION ( 'NONE',  ( 1.000000000000000000, 0.000000000000000000, 0.000000000000000000 ) ) ;
#7985 = CARTESIAN_POINT ( 'NONE',  ( 0.000000000000000000, -5.404747904883309660E-14, 15.47981323787947794 ) ) ;
#7986 = DIRECTION ( 'NONE',  ( 0.02857142857142857401, -0.9995917534020515305, 0.000000000000000000 ) ) ;
#7987 = VECTOR ( 'NONE', #7804, 1000.000000000000000 ) ;
#7988 = EDGE_CURVE ( 'NONE', #4008, #8012, #715, .T. ) ;
#7989 = CIRCLE ( 'NONE', #10687, 24.12539914357697768 ) ;
#7990 = LINE ( 'NONE', #10072, #12747 ) ;
#7991 = DIRECTION ( 'NONE',  ( -1.000000000000000000, 0.000000000000000000, -0.000000000000000000 ) ) ;
#7992 = ORIENTED_EDGE ( 'NONE', *, *, #4307, .F. ) ;
#7993 = DIRECTION ( 'NONE',  ( 0.000000000000000000, 0.000000000000000000, -1.000000000000000000 ) ) ;
#7994 = PRODUCT_DEFINITION_SHAPE ( 'NONE', 'NONE',  #15243 ) ;
#7995 = CARTESIAN_POINT ( 'NONE',  ( 86.00000000000000000, 0.000000000000000000, 4.500000000000000888 ) ) ;
#7996 = VERTEX_POINT ( 'NONE', #12545 ) ;
#7997 = AXIS2_PLACEMENT_3D ( 'NONE', #10251, #3327, #13781 ) ;
#7998 = ORIENTED_EDGE ( 'NONE', *, *, #8016, .T. ) ;
#7999 = VERTEX_POINT ( 'NONE', #12312 ) ;
#8000 = EDGE_LOOP ( 'NONE', ( #355, #89, #5868, #8665 ) ) ;
#8001 = CARTESIAN_POINT ( 'NONE',  ( 1.749999999999999778, 0.000000000000000000, 0.000000000000000000 ) ) ;
#8002 = CARTESIAN_POINT ( 'NONE',  ( 0.02436607992775717893, -9.836394144775869819, 22.71065055754449347 ) ) ;
#8003 = UNCERTAINTY_MEASURE_WITH_UNIT (LENGTH_MEASURE( 1.000000000000000082E-05 ), #961, 'distance_accuracy_value', 'NONE');
#8004 = CARTESIAN_POINT ( 'NONE',  ( 2.262072637928882468, -12.96450951081233605, 23.73240184472491876 ) ) ;
#8005 = VECTOR ( 'NONE', #12354, 1000.000000000000000 ) ;
#8006 = ORIENTED_EDGE ( 'NONE', *, *, #2726, .F. ) ;
#8007 = CARTESIAN_POINT ( 'NONE',  ( 1.749999999999999778, -12.83329210556822453, -12.55714665600001290 ) ) ;
#8008 = AXIS2_PLACEMENT_3D ( 'NONE', #13255, #12020, #9721 ) ;
#8009 = CARTESIAN_POINT ( 'NONE',  ( 2.789999999999999147, 22.71065055754452544, 9.836394144775786330 ) ) ;
#8010 = DIRECTION ( 'NONE',  ( 1.000000000000000000, 0.000000000000000000, 0.000000000000000000 ) ) ;
#8011 = CIRCLE ( 'NONE', #12169, 4.000000000000000888 ) ;
#8012 = VERTEX_POINT ( 'NONE', #13623 ) ;
#8013 = DIRECTION ( 'NONE',  ( 0.000000000000000000, 0.000000000000000000, 1.000000000000000000 ) ) ;
#8014 = CIRCLE ( 'NONE', #9249, 17.95481323787947758 ) ;
#8015 = DIRECTION ( 'NONE',  ( 1.000000000000000000, 0.000000000000000000, 0.000000000000000000 ) ) ;
#8016 = EDGE_CURVE ( 'NONE', #14530, #11965, #330, .T. ) ;
#8017 = ORIENTED_EDGE ( 'NONE', *, *, #14660, .F. ) ;
#8018 = EDGE_LOOP ( 'NONE', ( #9621, #3241, #6584, #4916 ) ) ;
#8019 = VECTOR ( 'NONE', #5664, 1000.000000000000000 ) ;
#8020 = DIRECTION ( 'NONE',  ( 0.000000000000000000, 0.000000000000000000, 1.000000000000000000 ) ) ;
#8021 = ORIENTED_EDGE ( 'NONE', *, *, #4103, .F. ) ;
#8022 = AXIS2_PLACEMENT_3D ( 'NONE', #9730, #13262, #12180 ) ;
#8023 = DIRECTION ( 'NONE',  ( -1.000000000000000000, -0.000000000000000000, -0.000000000000000000 ) ) ;
#8024 = DIRECTION ( 'NONE',  ( -5.480158469902919838E-17, -1.051478716308701618E-16, -1.000000000000000000 ) ) ;
#8025 =( REPRESENTATION_RELATIONSHIP ('NONE','NONE', #12685, #10044 ) REPRESENTATION_RELATIONSHIP_WITH_TRANSFORMATION ( #9494 )SHAPE_REPRESENTATION_RELATIONSHIP( ) );
#8026 = EDGE_CURVE ( 'NONE', #1275, #14803, #1817, .T. ) ;
#8027 = CARTESIAN_POINT ( 'NONE',  ( 2.789999999999999147, 23.48180575137737947, -5.535312321042476391 ) ) ;
#8028 = CARTESIAN_POINT ( 'NONE',  ( 80.00000000000000000, 0.000000000000000000, 4.500000000000003553 ) ) ;
#8029 = AXIS2_PLACEMENT_3D ( 'NONE', #4072, #9987, #14689 ) ;
#8030 = EDGE_LOOP ( 'NONE', ( #14632, #12462, #73, #1292, #7975, #8407 ) ) ;
#8031 = CIRCLE ( 'NONE', #13925, 2.524999999999997691 ) ;
#8032 = CYLINDRICAL_SURFACE ( 'NONE', #2388, 2.524999999999995914 ) ;
#8033 = ADVANCED_FACE ( 'NONE', ( #2948 ), #7636, .T. ) ;
#8034 = CARTESIAN_POINT ( 'NONE',  ( 8.000000000000000000, 0.000000000000000000, 0.000000000000000000 ) ) ;
#8035 = CIRCLE ( 'NONE', #3377, 14.01039946648074341 ) ;
#8036 = EDGE_LOOP ( 'NONE', ( #11690, #11703, #14829, #830 ) ) ;
#8037 = EDGE_CURVE ( 'NONE', #2008, #6501, #10164, .T. ) ;
#8038 = EDGE_LOOP ( 'NONE', ( #2813, #12996, #2436, #11499, #12412, #10738, #11838, #702, #12781, #12205, #15157, #10074, #597, #7438, #174, #11612, #10781, #10721, #1960, #3658, #12776, #12227, #5065, #1898, #2783, #8662, #7754, #5549, #2944, #9995, #13057, #9618, #7679, #9263, #9025, #1812, #13457, #6242, #10605, #11055, #8342, #14079, #4501, #7889, #6072 ) ) ;
#8039 = CARTESIAN_POINT ( 'NONE',  ( -7.810937420967753123E-14, 20.85287692521929159, 12.51293083811806461 ) ) ;
#8040 = DIRECTION ( 'NONE',  ( -1.000000000000000000, -0.000000000000000000, 0.000000000000000000 ) ) ;
#8041 = AXIS2_PLACEMENT_3D ( 'NONE', #5378, #7893, #13732 ) ;
#8042 = CARTESIAN_POINT ( 'NONE',  ( 0.000000000000000000, -23.48180575137736170, 5.535312321042622052 ) ) ;
#8043 = DIRECTION ( 'NONE',  ( 0.000000000000000000, 0.000000000000000000, 1.000000000000000000 ) ) ;
#8044 = AXIS2_PLACEMENT_3D ( 'NONE', #8117, #10641, #1265 ) ;
#8045 = CARTESIAN_POINT ( 'NONE',  ( 0.000000000000000000, 0.000000000000000000, 0.000000000000000000 ) ) ;
#8046 = AXIS2_PLACEMENT_3D ( 'NONE', #8583, #13192, #8728 ) ;
#8047 = AXIS2_PLACEMENT_3D ( 'NONE', #4843, #12970, #10319 ) ;
#8048 = CARTESIAN_POINT ( 'NONE',  ( 2.337784062669522989, 3.429166897524429825, 16.32199768300080933 ) ) ;
#8049 = EDGE_CURVE ( 'NONE', #13244, #12675, #2020, .T. ) ;
#8050 = ORIENTED_EDGE ( 'NONE', *, *, #11352, .T. ) ;
#8051 = CARTESIAN_POINT ( 'NONE',  ( 2.783068888626321513, 22.53293026234517171, -9.685942809246819607 ) ) ;
#8052 = EDGE_CURVE ( 'NONE', #5611, #6969, #7476, .T. ) ;
#8053 = CYLINDRICAL_SURFACE ( 'NONE', #14544, 17.95481323787947403 ) ;
#8054 = FACE_OUTER_BOUND ( 'NONE', #11674, .T. ) ;
#8055 = DIRECTION ( 'NONE',  ( 1.000000000000000000, 0.000000000000000000, 0.000000000000000000 ) ) ;
#8056 = ORIENTED_EDGE ( 'NONE', *, *, #6386, .F. ) ;
#8057 = LINE ( 'NONE', #13248, #7532 ) ;
#8058 = FACE_OUTER_BOUND ( 'NONE', #1481, .T. ) ;
#8059 = ORIENTED_EDGE ( 'NONE', *, *, #13418, .F. ) ;
#8060 = AXIS2_PLACEMENT_3D ( 'NONE', #7352, #8637, #13254 ) ;
#8061 = ORIENTED_EDGE ( 'NONE', *, *, #6548, .F. ) ;
#8062 = CARTESIAN_POINT ( 'NONE',  ( 2.262072769566604524, -24.43806413951684320, 11.57956866523208461 ) ) ;
#8063 = CARTESIAN_POINT ( 'NONE',  ( 1.749999999999998002, -4.633866840649122132, 27.68468304288257542 ) ) ;
#8064 = ORIENTED_EDGE ( 'NONE', *, *, #5019, .F. ) ;
#8065 = CARTESIAN_POINT ( 'NONE',  ( 0.007327532539344703763, -14.24942254254691143, 2.217238903388513371 ) ) ;
#8066 = DIRECTION ( 'NONE',  ( 0.000000000000000000, 0.000000000000000000, -1.000000000000000000 ) ) ;
#8067 = PLANE ( 'NONE',  #794 ) ;
#8068 = EDGE_CURVE ( 'NONE', #406, #799, #631, .T. ) ;
#8069 = CARTESIAN_POINT ( 'NONE',  ( 0.007349531976027265379, 2.217353748342130615, -14.24968354755766420 ) ) ;
#8070 = DIRECTION ( 'NONE',  ( 0.000000000000000000, 0.000000000000000000, 1.000000000000000000 ) ) ;
#8071 = EDGE_CURVE ( 'NONE', #8563, #5508, #13086, .T. ) ;
#8072 = EDGE_CURVE ( 'NONE', #12913, #2534, #11285, .T. ) ;
#8073 = EDGE_LOOP ( 'NONE', ( #5474, #659, #10560, #2403 ) ) ;
#8074 = DIRECTION ( 'NONE',  ( -1.000000000000000000, -0.000000000000000000, -0.000000000000000000 ) ) ;
#8075 = AXIS2_PLACEMENT_3D ( 'NONE', #11456, #933, #6776 ) ;
#8076 = CIRCLE ( 'NONE', #4396, 28.06981291497571362 ) ;
#8077 = DIRECTION ( 'NONE',  ( 0.000000000000000000, 0.000000000000000000, 1.000000000000000000 ) ) ;
#8078 = VERTEX_POINT ( 'NONE', #549 ) ;
#8079 = SURFACE_STYLE_FILL_AREA ( #1003 ) ;
#8080 = ORIENTED_EDGE ( 'NONE', *, *, #1667, .T. ) ;
#8081 = ORIENTED_EDGE ( 'NONE', *, *, #6384, .T. ) ;
#8082 = ORIENTED_EDGE ( 'NONE', *, *, #4480, .T. ) ;
#8083 = CARTESIAN_POINT ( 'NONE',  ( 0.000000000000000000, 0.000000000000000000, -0.8000000000000000444 ) ) ;
#8084 = DIRECTION ( 'NONE',  ( -0.000000000000000000, -0.000000000000000000, 1.000000000000000000 ) ) ;
#8085 = B_SPLINE_CURVE_WITH_KNOTS ( 'NONE', 3,
 ( #374, #5093, #8224, #14228, #13051, #2540, #13223, #1303 ),
 .UNSPECIFIED., .F., .F.,
 ( 4, 2, 2, 4 ),
 ( 2.445728210242702351E-07, 0.001895260649874686140, 0.002842768688401515337, 0.003790276726928345184 ),
 .UNSPECIFIED. ) ;
#8086 = CARTESIAN_POINT ( 'NONE',  ( 1.039999999999997815, -12.55714665599996316, 12.83329210556827604 ) ) ;
#8087 = CARTESIAN_POINT ( 'NONE',  ( 2.789999999999999147, -19.91106274590503844, -14.18181402625762821 ) ) ;
#8088 = TOROIDAL_SURFACE ( 'NONE', #1455, 14.01039946648074341, 8.000000000000000000 ) ;
#8089 = B_SPLINE_CURVE_WITH_KNOTS ( 'NONE', 3,
 ( #8890, #12349, #7967, #7828, #12513, #2131, #5454, #754 ),
 .UNSPECIFIED., .F., .F.,
 ( 4, 2, 2, 4 ),
 ( 4.663089412828908672E-07, 0.001898630173449110652, 0.002847712105703028435, 0.003796794037956946651 ),
 .UNSPECIFIED. ) ;
#8090 = LINE ( 'NONE', #709, #13242 ) ;
#8091 = EDGE_LOOP ( 'NONE', ( #8470, #9520, #9677, #13561, #14686, #9289 ) ) ;
#8092 = DIRECTION ( 'NONE',  ( 1.000000000000000000, -6.245004513516508695E-15, 0.000000000000000000 ) ) ;
#8093 = AXIS2_PLACEMENT_3D ( 'NONE', #5322, #14694, #8837 ) ;
#8094 = CARTESIAN_POINT ( 'NONE',  ( 0.2076373213218624669, 15.57879356040245078, -2.899259574942687046 ) ) ;
#8095 = EDGE_CURVE ( 'NONE', #1504, #6698, #1326, .T. ) ;
#8096 = ORIENTED_EDGE ( 'NONE', *, *, #12758, .F. ) ;
#8097 = CARTESIAN_POINT ( 'NONE',  ( -19.40394475573012301, -16.79473832354794993, 16.99999999999999645 ) ) ;
#8098 = LINE ( 'NONE', #9169, #10917 ) ;
#8099 = ORIENTED_EDGE ( 'NONE', *, *, #6386, .T. ) ;
#8100 = VERTEX_POINT ( 'NONE', #11981 ) ;
#8101 = CARTESIAN_POINT ( 'NONE',  ( 2.789999999999999147, 7.334849878007507762, 23.31896751603335005 ) ) ;
#8102 = AXIS2_PLACEMENT_3D ( 'NONE', #13808, #4144, #8817 ) ;
#8103 = ORIENTED_EDGE ( 'NONE', *, *, #8336, .F. ) ;
#8104 = FACE_OUTER_BOUND ( 'NONE', #11973, .T. ) ;
#8105 = CARTESIAN_POINT ( 'NONE',  ( 2.789999999999999147, 7.739906618939707883, 13.40591150984229252 ) ) ;
#8106 = EDGE_CURVE ( 'NONE', #13077, #12416, #14596, .T. ) ;
#8107 = CARTESIAN_POINT ( 'NONE',  ( -10.00000000000000000, 0.000000000000000000, 0.000000000000000000 ) ) ;
#8108 = CARTESIAN_POINT ( 'NONE',  ( 2.789999999999999147, -20.70663861606260170, -15.04425356660783031 ) ) ;
#8109 = VERTEX_POINT ( 'NONE', #10909 ) ;
#8110 = CARTESIAN_POINT ( 'NONE',  ( -1.149999999999998135, 0.000000000000000000, 0.000000000000000000 ) ) ;
#8111 = DIRECTION ( 'NONE',  ( -1.000000000000000000, 0.000000000000000000, 0.000000000000000000 ) ) ;
#8112 = ORIENTED_EDGE ( 'NONE', *, *, #15174, .F. ) ;
#8113 = ORIENTED_EDGE ( 'NONE', *, *, #6452, .T. ) ;
#8114 = LINE ( 'NONE', #12936, #2659 ) ;
#8115 = CARTESIAN_POINT ( 'NONE',  ( 2.789679245949058917, 20.70663861606308487, -12.51925356660738053 ) ) ;
#8116 = EDGE_CURVE ( 'NONE', #11849, #7839, #221, .T. ) ;
#8117 = CARTESIAN_POINT ( 'NONE',  ( 2.789999999999999147, -14.19996452731185776, -4.595504208220178022 ) ) ;
#8118 = FACE_OUTER_BOUND ( 'NONE', #9083, .T. ) ;
#8119 = CARTESIAN_POINT ( 'NONE',  ( 2.765633920072239071, -16.37294372382844543, -18.55949924794910544 ) ) ;
#8120 = EDGE_CURVE ( 'NONE', #6398, #3345, #10898, .T. ) ;
#8121 = LINE ( 'NONE', #10579, #1235 ) ;
#8122 = ORIENTED_EDGE ( 'NONE', *, *, #4652, .T. ) ;
#8123 = CARTESIAN_POINT ( 'NONE',  ( 2.789999999999999147, 22.71065055754465689, -9.836394144775473691 ) ) ;
#8124 = CARTESIAN_POINT ( 'NONE',  ( 1.749999999999999778, 0.000000000000000000, 0.000000000000000000 ) ) ;
#8125 = CARTESIAN_POINT ( 'NONE',  ( -0.2000000000000000111, -6.997142273814360713, 0.000000000000000000 ) ) ;
#8126 = CYLINDRICAL_SURFACE ( 'NONE', #15162, 5.400000000000000355 ) ;
#8127 = VERTEX_POINT ( 'NONE', #4940 ) ;
#8128 = DIRECTION ( 'NONE',  ( -0.9728364810787193395, -0.2314933715733012709, 0.000000000000000000 ) ) ;
#8129 = CARTESIAN_POINT ( 'NONE',  ( 2.236220367026671152, -16.15122426806985345, -5.139875429512027694 ) ) ;
#8130 = ORIENTED_EDGE ( 'NONE', *, *, #8615, .T. ) ;
#8131 = CARTESIAN_POINT ( 'NONE',  ( 14.40394475573011945, -10.79473832354794460, 22.47056274847713908 ) ) ;
#8132 = CARTESIAN_POINT ( 'NONE',  ( 33.82574562093736859, -6.697933970950280091, 2.999999999999999112 ) ) ;
#8133 = DIRECTION ( 'NONE',  ( 0.000000000000000000, 0.000000000000000000, 1.000000000000000000 ) ) ;
#8134 = FACE_OUTER_BOUND ( 'NONE', #3146, .T. ) ;
#8135 = DIRECTION ( 'NONE',  ( 0.000000000000000000, 0.000000000000000000, -1.000000000000000000 ) ) ;
#8136 = DIRECTION ( 'NONE',  ( -0.000000000000000000, -0.000000000000000000, 1.000000000000000000 ) ) ;
#8137 = CARTESIAN_POINT ( 'NONE',  ( 1.039999999999997593, 0.000000000000000000, 0.000000000000000000 ) ) ;
#8138 = ORIENTED_EDGE ( 'NONE', *, *, #6958, .F. ) ;
#8139 = FACE_OUTER_BOUND ( 'NONE', #2602, .T. ) ;
#8140 = ADVANCED_FACE ( 'NONE', ( #8531 ), #1767, .T. ) ;
#8141 = CARTESIAN_POINT ( 'NONE',  ( 0.000000000000000000, 0.000000000000000000, -0.8000000000000000444 ) ) ;
#8142 = ORIENTED_EDGE ( 'NONE', *, *, #11623, .F. ) ;
#8143 = FILL_AREA_STYLE ('',( #4770 ) ) ;
#8144 = ORIENTED_EDGE ( 'NONE', *, *, #10596, .F. ) ;
#8145 = ORIENTED_EDGE ( 'NONE', *, *, #9159, .F. ) ;
#8146 = ORIENTED_EDGE ( 'NONE', *, *, #2015, .T. ) ;
#8147 = DIRECTION ( 'NONE',  ( -1.000000000000000000, 0.000000000000000000, 0.000000000000000000 ) ) ;
#8148 = EDGE_CURVE ( 'NONE', #4678, #13200, #12119, .T. ) ;
#8149 = DIRECTION ( 'NONE',  ( 0.000000000000000000, -1.000000000000000000, 0.000000000000000000 ) ) ;
#8150 = EDGE_CURVE ( 'NONE', #9201, #10080, #14946, .T. ) ;
#8151 = AXIS2_PLACEMENT_3D ( 'NONE', #32, #10512, #11724 ) ;
#8152 = CARTESIAN_POINT ( 'NONE',  ( 0.2818302809372403850, -10.58084377126614584, -12.18203740414278258 ) ) ;
#8153 = FACE_OUTER_BOUND ( 'NONE', #11862, .T. ) ;
#8154 = DIRECTION ( 'NONE',  ( 0.000000000000000000, 0.000000000000000000, 1.000000000000000000 ) ) ;
#8155 = EDGE_LOOP ( 'NONE', ( #4722, #2466, #9128, #15107 ) ) ;
#8156 = CARTESIAN_POINT ( 'NONE',  ( 0.000000000000000000, 0.000000000000000000, -2.000000000000000000 ) ) ;
#8157 = CIRCLE ( 'NONE', #1535, 24.12539914357697413 ) ;
#8158 = VECTOR ( 'NONE', #13792, 1000.000000000000000 ) ;
#8159 = EDGE_CURVE ( 'NONE', #15027, #108, #7396, .T. ) ;
#8160 = ADVANCED_FACE ( 'NONE', ( #3846 ), #10403, .T. ) ;
#8161 = ORIENTED_EDGE ( 'NONE', *, *, #9330, .F. ) ;
#8162 = CARTESIAN_POINT ( 'NONE',  ( 1.749999999999999778, 4.835383649608716361, -17.29145405592683815 ) ) ;
#8163 = LINE ( 'NONE', #14009, #13624 ) ;
#8164 = EDGE_CURVE ( 'NONE', #1885, #8254, #2571, .T. ) ;
#8165 = ORIENTED_EDGE ( 'NONE', *, *, #1489, .T. ) ;
#8166 = ORIENTED_EDGE ( 'NONE', *, *, #4051, .T. ) ;
#8167 = AXIS2_PLACEMENT_3D ( 'NONE', #3421, #11781, #9400 ) ;
#8168 = DIRECTION ( 'NONE',  ( -1.000000000000000000, -0.000000000000000000, -0.000000000000000000 ) ) ;
#8169 = EDGE_CURVE ( 'NONE', #6501, #3521, #8449, .T. ) ;
#8170 = ORIENTED_EDGE ( 'NONE', *, *, #6839, .T. ) ;
#8171 = CARTESIAN_POINT ( 'NONE',  ( 1.249999999999997558, 0.000000000000000000, 0.000000000000000000 ) ) ;
#8172 = DIRECTION ( 'NONE',  ( 1.000000000000000000, 0.000000000000000000, 0.000000000000000000 ) ) ;
#8173 = FACE_OUTER_BOUND ( 'NONE', #2407, .T. ) ;
#8174 = CARTESIAN_POINT ( 'NONE',  ( 2.789999999999999147, -5.535312321042889394, 23.48180575137727999 ) ) ;
#8175 = ORIENTED_EDGE ( 'NONE', *, *, #9192, .T. ) ;
#8176 = CARTESIAN_POINT ( 'NONE',  ( 0.000000000000000000, -15.74360496233370021, -18.28042085475294698 ) ) ;
#8177 = LINE ( 'NONE', #1192, #4097 ) ;
#8178 = ORIENTED_EDGE ( 'NONE', *, *, #2129, .T. ) ;
#8179 = ORIENTED_EDGE ( 'NONE', *, *, #12328, .T. ) ;
#8180 = ADVANCED_BREP_SHAPE_REPRESENTATION ( '', ( #8383, #1376 ), #2126 ) ;
#8181 = CARTESIAN_POINT ( 'NONE',  ( 0.2818303916520942254, -5.259531939870306871, 15.25429862889480148 ) ) ;
#8182 = FACE_OUTER_BOUND ( 'NONE', #7514, .T. ) ;
#8183 = CARTESIAN_POINT ( 'NONE',  ( 1.749999999999999778, 4.835383649608472112, 17.29145405592690210 ) ) ;
#8184 = DIRECTION ( 'NONE',  ( -1.000000000000000000, -0.000000000000000000, -0.000000000000000000 ) ) ;
#8185 = CARTESIAN_POINT ( 'NONE',  ( 0.000000000000000000, 11.04103753892271733, 8.624777288397844188 ) ) ;
#8186 = CARTESIAN_POINT ( 'NONE',  ( 13.28797974610715116, -21.11867004231547540, 7.000000000000000000 ) ) ;
#8187 = EDGE_CURVE ( 'NONE', #6211, #9602, #4292, .T. ) ;
#8188 = VERTEX_POINT ( 'NONE', #6455 ) ;
#8189 = CYLINDRICAL_SURFACE ( 'NONE', #10034, 6.000000000000005329 ) ;
#8190 = CARTESIAN_POINT ( 'NONE',  ( 0.5321745379877897975, -12.96514671151783915, 23.74442027961355706 ) ) ;
#8191 = CARTESIAN_POINT ( 'NONE',  ( 0.000000000000000000, 5.249430348645754307, 12.98979500319696534 ) ) ;
#8192 = DIRECTION ( 'NONE',  ( 1.000000000000000000, 0.000000000000000000, 0.000000000000000000 ) ) ;
#8193 = DIRECTION ( 'NONE',  ( -0.000000000000000000, -0.000000000000000000, 1.000000000000000000 ) ) ;
#8194 = ORIENTED_EDGE ( 'NONE', *, *, #5998, .T. ) ;
#8195 = EDGE_LOOP ( 'NONE', ( #11263, #12072, #5164, #177 ) ) ;
#8196 = VECTOR ( 'NONE', #239, 999.9999999999998863 ) ;
#8197 = ORIENTED_EDGE ( 'NONE', *, *, #10499, .F. ) ;
#8198 = CIRCLE ( 'NONE', #11874, 4.000000000000003553 ) ;
#8199 = DIRECTION ( 'NONE',  ( -0.000000000000000000, -0.000000000000000000, -1.000000000000000000 ) ) ;
#8200 = FACE_OUTER_BOUND ( 'NONE', #6974, .T. ) ;
#8201 = DIRECTION ( 'NONE',  ( -0.4055247608874392173, 0.9140840597599245720, -7.389059384413459453E-17 ) ) ;
#8202 = CARTESIAN_POINT ( 'NONE',  ( 2.764680872515352661, 9.232963481057920418, -11.36963888406677725 ) ) ;
#8203 = CARTESIAN_POINT ( 'NONE',  ( 0.02436607992776498519, -21.30679549418621832, -12.59161484032935618 ) ) ;
#8204 = DIRECTION ( 'NONE',  ( -1.000000000000000000, -0.000000000000000000, -0.000000000000000000 ) ) ;
#8205 = DIRECTION ( 'NONE',  ( 1.000000000000000000, 0.000000000000000000, 0.000000000000000000 ) ) ;
#8206 = VECTOR ( 'NONE', #4620, 1000.000000000000000 ) ;
#8207 = ORIENTED_EDGE ( 'NONE', *, *, #842, .T. ) ;
#8208 = CYLINDRICAL_SURFACE ( 'NONE', #5082, 3.000000000000002665 ) ;
#8209 = CIRCLE ( 'NONE', #12133, 2.524999999999997691 ) ;
#8210 = AXIS2_PLACEMENT_3D ( 'NONE', #12889, #10603, #5850 ) ;
#8211 = CARTESIAN_POINT ( 'NONE',  ( -7.770166132776744975E-14, -12.51293083811813389, 20.85287692521926672 ) ) ;
#8212 = ORIENTED_EDGE ( 'NONE', *, *, #8495, .F. ) ;
#8213 = EDGE_CURVE ( 'NONE', #12316, #15059, #2320, .T. ) ;
#8214 = AXIS2_PLACEMENT_3D ( 'NONE', #10888, #1447, #353 ) ;
#8215 = ORIENTED_EDGE ( 'NONE', *, *, #2032, .T. ) ;
#8216 = ORIENTED_EDGE ( 'NONE', *, *, #11905, .F. ) ;
#8217 = ORIENTED_EDGE ( 'NONE', *, *, #14598, .F. ) ;
#8218 = FACE_BOUND ( 'NONE', #12969, .T. ) ;
#8219 = CIRCLE ( 'NONE', #6260, 4.000000000000000000 ) ;
#8220 = CARTESIAN_POINT ( 'NONE',  ( -9.999999999999992895, -25.00000000000000000, 4.000000000000003553 ) ) ;
#8221 = VECTOR ( 'NONE', #1711, 1000.000000000000227 ) ;
#8222 = ADVANCED_FACE ( 'NONE', ( #7543 ), #858, .T. ) ;
#8223 = LINE ( 'NONE', #12898, #6089 ) ;
#8224 = CARTESIAN_POINT ( 'NONE',  ( 2.597943782557558645, -10.28947301956273996, -12.05486625177582560 ) ) ;
#8225 = DIRECTION ( 'NONE',  ( -0.000000000000000000, -0.000000000000000000, -1.000000000000000000 ) ) ;
#8226 = ORIENTED_EDGE ( 'NONE', *, *, #13779, .F. ) ;
#8227 = CARTESIAN_POINT ( 'NONE',  ( 2.789999999999999147, 13.68080036884348516, 5.229914364928400339 ) ) ;
#8228 = EDGE_CURVE ( 'NONE', #7557, #11633, #11148, .T. ) ;
#8229 = CIRCLE ( 'NONE', #7997, 2.524999999999999467 ) ;
#8230 = EDGE_CURVE ( 'NONE', #228, #212, #5176, .T. ) ;
#8231 = B_SPLINE_CURVE_WITH_KNOTS ( 'NONE', 3,
 ( #6360, #8586, #11043, #1820, #9886, #14585 ),
 .UNSPECIFIED., .F., .F.,
 ( 4, 2, 4 ),
 ( 4.462636678112536814E-07, 0.001879885020955181143, 0.003759323778242551310 ),
 .UNSPECIFIED. ) ;
#8232 = ORIENTED_EDGE ( 'NONE', *, *, #1768, .F. ) ;
#8233 = CARTESIAN_POINT ( 'NONE',  ( 3.948182771089140175, -23.68909662653485171, 4.000000000000000000 ) ) ;
#8234 = CARTESIAN_POINT ( 'NONE',  ( 0.000000000000000000, 0.000000000000000000, 0.000000000000000000 ) ) ;
#8235 = VERTEX_POINT ( 'NONE', #14607 ) ;
#8236 = ORIENTED_EDGE ( 'NONE', *, *, #5994, .T. ) ;
#8237 = CIRCLE ( 'NONE', #10693, 4.999999999999997335 ) ;
#8238 = CARTESIAN_POINT ( 'NONE',  ( 2.765633920072236851, -22.71065055754445439, -9.836394144775947979 ) ) ;
#8239 = EDGE_CURVE ( 'NONE', #11238, #4224, #2928, .T. ) ;
#8240 = VERTEX_POINT ( 'NONE', #8447 ) ;
#8241 = CARTESIAN_POINT ( 'NONE',  ( 0.000000000000000000, 13.87420763704361626, 1.948757464274225137 ) ) ;
#8242 = CARTESIAN_POINT ( 'NONE',  ( 80.82762530298222714, -19.99999999999999645, -131.1575142076926852 ) ) ;
#8243 = EDGE_CURVE ( 'NONE', #1849, #7933, #11637, .T. ) ;
#8244 = DIRECTION ( 'NONE',  ( -0.000000000000000000, -0.000000000000000000, 1.000000000000000000 ) ) ;
#8245 = VECTOR ( 'NONE', #10223, 1000.000000000000000 ) ;
#8246 = CYLINDRICAL_SURFACE ( 'NONE', #8686, 2.524999999999995914 ) ;
#8247 = ORIENTED_EDGE ( 'NONE', *, *, #3988, .T. ) ;
#8248 = VECTOR ( 'NONE', #13282, 1000.000000000000114 ) ;
#8249 = DIRECTION ( 'NONE',  ( -0.000000000000000000, -0.000000000000000000, 1.000000000000000000 ) ) ;
#8250 = DIRECTION ( 'NONE',  ( 0.000000000000000000, 0.000000000000000000, -1.000000000000000000 ) ) ;
#8251 =( GEOMETRIC_REPRESENTATION_CONTEXT ( 3 ) GLOBAL_UNCERTAINTY_ASSIGNED_CONTEXT ( ( #391 ) ) GLOBAL_UNIT_ASSIGNED_CONTEXT ( ( #9778, #3939, #6392 ) ) REPRESENTATION_CONTEXT ( 'NONE', 'WORKASPACE' ) );
#8252 = ORIENTED_EDGE ( 'NONE', *, *, #7138, .T. ) ;
#8253 = EDGE_CURVE ( 'NONE', #1577, #6574, #14997, .T. ) ;
#8254 = VERTEX_POINT ( 'NONE', #12527 ) ;
#8255 = CARTESIAN_POINT ( 'NONE',  ( 0.1920562174424399748, -12.05486625177564797, -10.28947301956294780 ) ) ;
#8256 = CARTESIAN_POINT ( 'NONE',  ( 2.780897501012522977, 21.10878525316979903, -12.54316204260869760 ) ) ;
#8257 = VECTOR ( 'NONE', #9754, 1000.000000000000000 ) ;
#8258 = AXIS2_PLACEMENT_3D ( 'NONE', #5245, #7468, #1625 ) ;
#8259 = CARTESIAN_POINT ( 'NONE',  ( 1.039999999999997593, -24.89775460606841051, 12.96210679857778025 ) ) ;
#8260 = DIRECTION ( 'NONE',  ( 0.000000000000000000, 0.000000000000000000, 1.000000000000000000 ) ) ;
#8261 = DIRECTION ( 'NONE',  ( -1.000000000000000000, -0.000000000000000000, -0.000000000000000000 ) ) ;
#8262 = CIRCLE ( 'NONE', #10239, 14.01039946648074341 ) ;
#8263 = FACE_BOUND ( 'NONE', #7318, .T. ) ;
#8264 = VECTOR ( 'NONE', #2904, 1000.000000000000000 ) ;
#8265 = EDGE_LOOP ( 'NONE', ( #7980, #11453, #11329, #6251 ) ) ;
#8266 = CARTESIAN_POINT ( 'NONE',  ( 2.257825477245772650, 19.66801664102704095, 18.57583492944426951 ) ) ;
#8267 = CARTESIAN_POINT ( 'NONE',  ( 2.141980652367355464, -6.189445006155633422, -0.8000000000000000444 ) ) ;
#8268 = CARTESIAN_POINT ( 'NONE',  ( 2.789999999999999147, 0.000000000000000000, 0.000000000000000000 ) ) ;
#8269 = CARTESIAN_POINT ( 'NONE',  ( -10.00000000000000000, 0.000000000000000000, 0.000000000000000000 ) ) ;
#8270 = ORIENTED_EDGE ( 'NONE', *, *, #8533, .T. ) ;
#8271 = ORIENTED_EDGE ( 'NONE', *, *, #13622, .F. ) ;
#8272 = ADVANCED_FACE ( 'NONE', ( #1927 ), #6617, .T. ) ;
#8273 = DIRECTION ( 'NONE',  ( 0.000000000000000000, 0.000000000000000000, -1.000000000000000000 ) ) ;
#8274 = ORIENTED_EDGE ( 'NONE', *, *, #6275, .F. ) ;
#8275 = TOROIDAL_SURFACE ( 'NONE', #167, 24.12539914357697768, 8.000000000000000000 ) ;
#8276 = CARTESIAN_POINT ( 'NONE',  ( 1.039999999999999369, 12.55714665599987079, 12.83329210556836308 ) ) ;
#8277 = DIRECTION ( 'NONE',  ( -1.000000000000000000, -0.000000000000000000, -0.000000000000000000 ) ) ;
#8278 = CIRCLE ( 'NONE', #10253, 4.999999999999997335 ) ;
#8279 = CIRCLE ( 'NONE', #956, 28.06981291497571362 ) ;
#8280 = CARTESIAN_POINT ( 'NONE',  ( 0.000000000000000000, 0.4273491293402468805, 0.000000000000000000 ) ) ;
#8281 = DIRECTION ( 'NONE',  ( -1.000000000000000000, -0.000000000000000000, -0.000000000000000000 ) ) ;
#8282 = DIRECTION ( 'NONE',  ( 0.000000000000000000, 0.000000000000000000, 1.000000000000000000 ) ) ;
#8283 = CARTESIAN_POINT ( 'NONE',  ( -1.000000000000000222, -4.808326913195983821, -0.8000000000000000444 ) ) ;
#8284 = ORIENTED_EDGE ( 'NONE', *, *, #8413, .T. ) ;
#8285 = CARTESIAN_POINT ( 'NONE',  ( 2.764680872513205934, -11.36963888406694068, 9.232963481057725019 ) ) ;
#8286 = CARTESIAN_POINT ( 'NONE',  ( -16.96657417111497068, -13.60061260430328467, 0.7999999999999960476 ) ) ;
#8287 = VERTEX_POINT ( 'NONE', #13825 ) ;
#8288 = FACE_OUTER_BOUND ( 'NONE', #14664, .T. ) ;
#8289 = CARTESIAN_POINT ( 'NONE',  ( 0.000000000000000000, 0.000000000000000000, 0.000000000000000000 ) ) ;
#8290 = VECTOR ( 'NONE', #10611, 1000.000000000000000 ) ;
#8291 = CYLINDRICAL_SURFACE ( 'NONE', #592, 8.400000000000000355 ) ;
#8292 = EDGE_CURVE ( 'NONE', #13868, #10903, #9816, .T. ) ;
#8293 = ORIENTED_EDGE ( 'NONE', *, *, #12074, .T. ) ;
#8294 = CIRCLE ( 'NONE', #9280, 14.01039946648073986 ) ;
#8295 = FILL_AREA_STYLE_COLOUR ( '', #11854 ) ;
#8296 = ORIENTED_EDGE ( 'NONE', *, *, #8888, .F. ) ;
#8297 = ORIENTED_EDGE ( 'NONE', *, *, #13799, .F. ) ;
#8298 = EDGE_LOOP ( 'NONE', ( #88, #7255, #4568, #5031 ) ) ;
#8299 = FACE_BOUND ( 'NONE', #5038, .T. ) ;
#8300 = CARTESIAN_POINT ( 'NONE',  ( 2.765633920072233742, -24.15498966839966855, 5.391175441198523544 ) ) ;
#8301 = DIRECTION ( 'NONE',  ( 0.000000000000000000, 0.000000000000000000, 1.000000000000000000 ) ) ;
#8302 = CARTESIAN_POINT ( 'NONE',  ( 2.582362678678087331, -2.899259574942854023, 15.57879356040262309 ) ) ;
#8303 = EDGE_CURVE ( 'NONE', #3308, #3757, #913, .T. ) ;
#8304 = DIRECTION ( 'NONE',  ( -1.000000000000000000, -0.000000000000000000, 0.000000000000000000 ) ) ;
#8305 = AXIS2_PLACEMENT_3D ( 'NONE', #2798, #407, #7498 ) ;
#8306 = AXIS2_PLACEMENT_3D ( 'NONE', #14752, #6602, #4516 ) ;
#8307 = ADVANCED_FACE ( 'NONE', ( #12449 ), #10143, .T. ) ;
#8308 = EDGE_LOOP ( 'NONE', ( #9916, #7142, #10014, #743 ) ) ;
#8309 = CARTESIAN_POINT ( 'NONE',  ( 98.63205416320636232, -2.094184955359725375, 6.000000000000000000 ) ) ;
#8310 = APPLICATION_CONTEXT ( 'automotive_design' ) ;
#8311 = AXIS2_PLACEMENT_3D ( 'NONE', #3895, #565, #9876 ) ;
#8312 = AXIS2_PLACEMENT_3D ( 'NONE', #4575, #9396, #6948 ) ;
#8313 = ORIENTED_EDGE ( 'NONE', *, *, #2597, .F. ) ;
#8314 = AXIS2_PLACEMENT_3D ( 'NONE', #5742, #11569, #12864 ) ;
#8315 = CYLINDRICAL_SURFACE ( 'NONE', #12151, 2.447112362156698140 ) ;
#8316 = CARTESIAN_POINT ( 'NONE',  ( -1.398397006336996817, -6.091550361990593743, -0.8000000000000000444 ) ) ;
#8317 = ORIENTED_EDGE ( 'NONE', *, *, #12278, .T. ) ;
#8318 = ORIENTED_EDGE ( 'NONE', *, *, #4205, .T. ) ;
#8319 = EDGE_CURVE ( 'NONE', #5935, #799, #10297, .T. ) ;
#8320 = DIRECTION ( 'NONE',  ( -0.9237280213470681067, -0.3830490080632377725, 0.000000000000000000 ) ) ;
#8321 = ORIENTED_EDGE ( 'NONE', *, *, #15016, .T. ) ;
#8322 = DIRECTION ( 'NONE',  ( 1.000000000000000000, 0.000000000000000000, 0.000000000000000000 ) ) ;
#8323 = CARTESIAN_POINT ( 'NONE',  ( 80.82762530298222714, -9.999999999999994671, 7.000000000000000000 ) ) ;
#8324 = CIRCLE ( 'NONE', #6127, 4.000000000000000888 ) ;
#8325 = CARTESIAN_POINT ( 'NONE',  ( -4.872650870659752442, 0.4273491293402474911, -0.8000000000000000444 ) ) ;
#8326 = CARTESIAN_POINT ( 'NONE',  ( 2.646101151984011857, -14.59528211758545524, 5.279841123860813390 ) ) ;
#8327 = EDGE_CURVE ( 'NONE', #1528, #11073, #3314, .T. ) ;
#8328 = ORIENTED_EDGE ( 'NONE', *, *, #3116, .T. ) ;
#8329 = CARTESIAN_POINT ( 'NONE',  ( -6.000000000000000888, 7.347880794884120722E-16, 7.000000000000000000 ) ) ;
#8330 = FACE_OUTER_BOUND ( 'NONE', #12198, .T. ) ;
#8331 = VERTEX_POINT ( 'NONE', #14766 ) ;
#8332 = ORIENTED_EDGE ( 'NONE', *, *, #3716, .T. ) ;
#8333 = ORIENTED_EDGE ( 'NONE', *, *, #505, .T. ) ;
#8334 = FACE_BOUND ( 'NONE', #731, .T. ) ;
#8335 = CARTESIAN_POINT ( 'NONE',  ( -3.799999999999999378, 4.653657836759941744E-16, -0.8000000000000000444 ) ) ;
#8336 = EDGE_CURVE ( 'NONE', #11120, #10268, #6988, .T. ) ;
#8337 = ADVANCED_FACE ( 'NONE', ( #602, #8907 ), #5321, .T. ) ;
#8338 = CARTESIAN_POINT ( 'NONE',  ( -1.000000000000000222, -4.808326913195983821, 0.000000000000000000 ) ) ;
#8339 = CARTESIAN_POINT ( 'NONE',  ( 1.749999999999998002, 0.000000000000000000, 0.000000000000000000 ) ) ;
#8340 = CARTESIAN_POINT ( 'NONE',  ( 8.000000000000000000, 0.000000000000000000, 0.000000000000000000 ) ) ;
#8341 = CARTESIAN_POINT ( 'NONE',  ( 1.749999999999998002, -27.76164181293054511, 4.147968289691195132 ) ) ;
#8342 = ORIENTED_EDGE ( 'NONE', *, *, #5568, .F. ) ;
#8343 = CARTESIAN_POINT ( 'NONE',  ( 2.789999999999999147, 22.25075486061751207, -9.324097380959219805 ) ) ;
#8344 = DIRECTION ( 'NONE',  ( 0.000000000000000000, 0.000000000000000000, 1.000000000000000000 ) ) ;
#8345 = CYLINDRICAL_SURFACE ( 'NONE', #2374, 17.95481323787947403 ) ;
#8346 = ORIENTED_EDGE ( 'NONE', *, *, #11989, .T. ) ;
#8347 = EDGE_CURVE ( 'NONE', #7388, #3989, #14692, .T. ) ;
#8348 = ORIENTED_EDGE ( 'NONE', *, *, #11440, .F. ) ;
#8349 = EDGE_CURVE ( 'NONE', #1588, #5525, #5532, .T. ) ;
#8350 = VERTEX_POINT ( 'NONE', #13677 ) ;
#8351 = DIRECTION ( 'NONE',  ( 0.000000000000000000, 0.000000000000000000, 1.000000000000000000 ) ) ;
#8352 = CARTESIAN_POINT ( 'NONE',  ( 0.000000000000000000, 0.000000000000000000, 0.000000000000000000 ) ) ;
#8353 = EDGE_CURVE ( 'NONE', #2853, #1779, #1556, .T. ) ;
#8354 = LINE ( 'NONE', #6979, #13426 ) ;
#8355 = CARTESIAN_POINT ( 'NONE',  ( 0.02436607992776108206, -24.15498966839966855, 5.391175441198523544 ) ) ;
#8356 = DIRECTION ( 'NONE',  ( 0.000000000000000000, 0.000000000000000000, 1.000000000000000000 ) ) ;
#8357 = FACE_BOUND ( 'NONE', #10378, .T. ) ;
#8358 = VERTEX_POINT ( 'NONE', #3076 ) ;
#8359 = CYLINDRICAL_SURFACE ( 'NONE', #14984, 2.524999999999995914 ) ;
#8360 = EDGE_CURVE ( 'NONE', #14624, #8921, #9208, .T. ) ;
#8361 = EDGE_LOOP ( 'NONE', ( #6051, #9170, #6850, #13519 ) ) ;
#8362 = CARTESIAN_POINT ( 'NONE',  ( 0.000000000000000000, -20.70663861606282197, 15.04425356660753188 ) ) ;
#8363 = DIRECTION ( 'NONE',  ( 0.000000000000000000, 0.000000000000000000, 1.000000000000000000 ) ) ;
#8364 = PRODUCT_DEFINITION_SHAPE ( 'NONE', 'NONE',  #15234 ) ;
#8365 = ORIENTED_EDGE ( 'NONE', *, *, #1210, .F. ) ;
#8366 = ORIENTED_EDGE ( 'NONE', *, *, #109, .F. ) ;
#8367 = EDGE_LOOP ( 'NONE', ( #1312, #2697, #12223, #12430 ) ) ;
#8368 = ORIENTED_EDGE ( 'NONE', *, *, #4466, .F. ) ;
#8369 = DIRECTION ( 'NONE',  ( 0.000000000000000000, 0.000000000000000000, 1.000000000000000000 ) ) ;
#8370 = DIRECTION ( 'NONE',  ( -0.1643989873053574580, 0.9863939238321436376, 0.000000000000000000 ) ) ;
#8371 = CARTESIAN_POINT ( 'NONE',  ( 0.02531912748631424959, 14.46287784598617243, 2.311161484776605324 ) ) ;
#8372 = FACE_OUTER_BOUND ( 'NONE', #14734, .T. ) ;
#8373 = CARTESIAN_POINT ( 'NONE',  ( 2.783068961317271217, -12.53626894672843051, 21.08061549536610713 ) ) ;
#8374 = ORIENTED_EDGE ( 'NONE', *, *, #9310, .T. ) ;
#8375 = DIRECTION ( 'NONE',  ( 0.000000000000000000, 0.000000000000000000, 1.000000000000000000 ) ) ;
#8376 = CIRCLE ( 'NONE', #7917, 0.5999999999999998668 ) ;
#8377 = ORIENTED_EDGE ( 'NONE', *, *, #4698, .F. ) ;
#8378 = DIRECTION ( 'NONE',  ( 0.000000000000000000, 0.000000000000000000, 1.000000000000000000 ) ) ;
#8379 = EDGE_CURVE ( 'NONE', #10328, #10680, #2003, .T. ) ;
#8380 = FACE_OUTER_BOUND ( 'NONE', #11381, .T. ) ;
#8381 = ORIENTED_EDGE ( 'NONE', *, *, #11277, .T. ) ;
#8382 = VERTEX_POINT ( 'NONE', #5542 ) ;
#8383 = MANIFOLD_SOLID_BREP ( 'Boss-Extrude1', #7216 ) ;
#8384 = DIRECTION ( 'NONE',  ( -0.1643989873053572359, 0.9863939238321437486, 0.000000000000000000 ) ) ;
#8385 = ORIENTED_EDGE ( 'NONE', *, *, #14788, .F. ) ;
#8386 = VECTOR ( 'NONE', #736, 1000.000000000000000 ) ;
#8387 = DIRECTION ( 'NONE',  ( 1.000000000000000000, -0.000000000000000000, -0.000000000000000000 ) ) ;
#8388 = B_SPLINE_CURVE_WITH_KNOTS ( 'NONE', 3,
 ( #561, #5282, #13862, #14088, #9177, #10630 ),
 .UNSPECIFIED., .F., .F.,
 ( 4, 2, 4 ),
 ( 2.321268216997094965E-07, 0.001878622960950492287, 0.003757013795079284547 ),
 .UNSPECIFIED. ) ;
#8389 = CARTESIAN_POINT ( 'NONE',  ( 2.789999999999999147, 9.324097380959445402, 22.25075486061742325 ) ) ;
#8390 = DIRECTION ( 'NONE',  ( 0.000000000000000000, -1.000000000000000000, 0.000000000000000000 ) ) ;
#8391 = DIRECTION ( 'NONE',  ( -1.000000000000000000, -0.000000000000000000, -0.000000000000000000 ) ) ;
#8392 = ORIENTED_EDGE ( 'NONE', *, *, #5818, .F. ) ;
#8393 = CARTESIAN_POINT ( 'NONE',  ( 2.789999999999999147, -23.31896751603326834, -7.334849878007764445 ) ) ;
#8394 = DIRECTION ( 'NONE',  ( 0.9988110320138940956, 0.04874958797097353469, 0.000000000000000000 ) ) ;
#8395 = ORIENTED_EDGE ( 'NONE', *, *, #4802, .T. ) ;
#8396 = CARTESIAN_POINT ( 'NONE',  ( 2.789999999999999147, -24.04302995059966719, 1.991882183130210482 ) ) ;
#8397 = AXIS2_PLACEMENT_3D ( 'NONE', #8656, #9591, #6060 ) ;
#8398 = ORIENTED_EDGE ( 'NONE', *, *, #3432, .F. ) ;
#8399 = EDGE_LOOP ( 'NONE', ( #9584, #11962, #8978, #10332, #1728, #5368 ) ) ;
#8400 = CARTESIAN_POINT ( 'NONE',  ( 0.02436607992776411782, -24.63872515616084513, 2.336989772644183283 ) ) ;
#8401 = CARTESIAN_POINT ( 'NONE',  ( 0.000000000000000000, -23.48180575137727288, -5.535312321042949790 ) ) ;
#8402 = ADVANCED_FACE ( 'NONE', ( #12876 ), #2362, .T. ) ;
#8403 = CARTESIAN_POINT ( 'NONE',  ( 88.84370878116858705, 10.64188714589527507, -2.000000000000000888 ) ) ;
#8404 = DIRECTION ( 'NONE',  ( 1.000000000000000000, 0.000000000000000000, 0.000000000000000000 ) ) ;
#8405 = DIRECTION ( 'NONE',  ( 0.000000000000000000, 0.000000000000000000, 1.000000000000000000 ) ) ;
#8406 = CARTESIAN_POINT ( 'NONE',  ( 1.749999999999998002, 0.000000000000000000, 0.000000000000000000 ) ) ;
#8407 = ORIENTED_EDGE ( 'NONE', *, *, #13023, .F. ) ;
#8408 = DIRECTION ( 'NONE',  ( -1.000000000000000000, -0.000000000000000000, -0.000000000000000000 ) ) ;
#8409 = DIRECTION ( 'NONE',  ( -1.000000000000000000, -0.000000000000000000, -0.000000000000000000 ) ) ;
#8410 = FACE_OUTER_BOUND ( 'NONE', #5477, .T. ) ;
#8411 = DIRECTION ( 'NONE',  ( 0.000000000000000000, 0.000000000000000000, 1.000000000000000000 ) ) ;
#8412 = EDGE_CURVE ( 'NONE', #10155, #14530, #9717, .T. ) ;
#8413 = EDGE_CURVE ( 'NONE', #5313, #5535, #6180, .T. ) ;
#8414 = EDGE_CURVE ( 'NONE', #13214, #4401, #2104, .T. ) ;
#8415 = ORIENTED_EDGE ( 'NONE', *, *, #1758, .T. ) ;
#8416 = ORIENTED_EDGE ( 'NONE', *, *, #8836, .T. ) ;
#8417 = VERTEX_POINT ( 'NONE', #4609 ) ;
#8418 = CARTESIAN_POINT ( 'NONE',  ( 0.000000000000000000, 15.74360496233409634, -18.28042085475261302 ) ) ;
#8419 = DIRECTION ( 'NONE',  ( -0.000000000000000000, -0.000000000000000000, -1.000000000000000000 ) ) ;
#8420 = PLANE ( 'NONE',  #2872 ) ;
#8421 = DIRECTION ( 'NONE',  ( 1.000000000000000000, 0.000000000000000000, 0.000000000000000000 ) ) ;
#8422 = CARTESIAN_POINT ( 'NONE',  ( 80.00000000000001421, 1.084202172485504434E-16, -7.799999999999999822 ) ) ;
#8423 = DIRECTION ( 'NONE',  ( 0.000000000000000000, 0.000000000000000000, 1.000000000000000000 ) ) ;
#8424 = ORIENTED_EDGE ( 'NONE', *, *, #10840, .F. ) ;
#8425 = CARTESIAN_POINT ( 'NONE',  ( -1.149999999999998135, 0.000000000000000000, -4.100000000000000533 ) ) ;
#8426 = CARTESIAN_POINT ( 'NONE',  ( 0.5321745087963422050, -11.58891744060090367, -24.44564404695856297 ) ) ;
#8427 = EDGE_CURVE ( 'NONE', #10827, #159, #7424, .T. ) ;
#8428 = EDGE_CURVE ( 'NONE', #1826, #7716, #12083, .T. ) ;
#8429 = STYLED_ITEM ( 'NONE', ( #4932 ), #4912 ) ;
#8430 = ORIENTED_EDGE ( 'NONE', *, *, #5524, .T. ) ;
#8431 = CARTESIAN_POINT ( 'NONE',  ( 1.039999999999996927, 20.02152543075374069, -19.67366047555508501 ) ) ;
#8432 = CARTESIAN_POINT ( 'NONE',  ( 0.9041604711286044260, 12.27244837507631381, -12.77651625388886281 ) ) ;
#8433 = SURFACE_STYLE_FILL_AREA ( #10825 ) ;
#8434 = EDGE_CURVE ( 'NONE', #15013, #3736, #4792, .T. ) ;
#8435 = ORIENTED_EDGE ( 'NONE', *, *, #6769, .T. ) ;
#8436 = AXIS2_PLACEMENT_3D ( 'NONE', #6475, #1720, #11159 ) ;
#8437 = VECTOR ( 'NONE', #12780, 1000.000000000000000 ) ;
#8438 = TOROIDAL_SURFACE ( 'NONE', #10407, 14.01039946648074341, 8.000000000000000000 ) ;
#8439 = ORIENTED_EDGE ( 'NONE', *, *, #10755, .F. ) ;
#8440 = ORIENTED_EDGE ( 'NONE', *, *, #3827, .T. ) ;
#8441 = ORIENTED_EDGE ( 'NONE', *, *, #12147, .T. ) ;
#8442 = CYLINDRICAL_SURFACE ( 'NONE', #4596, 1.999999999999998446 ) ;
#8443 = DIRECTION ( 'NONE',  ( -1.000000000000000000, -0.000000000000000000, -0.000000000000000000 ) ) ;
#8444 = EDGE_CURVE ( 'NONE', #6351, #3683, #8209, .T. ) ;
#8445 = FACE_OUTER_BOUND ( 'NONE', #38, .T. ) ;
#8446 = CARTESIAN_POINT ( 'NONE',  ( 2.789999999999999147, 0.000000000000000000, 0.000000000000000000 ) ) ;
#8447 = CARTESIAN_POINT ( 'NONE',  ( -6.000000000000000888, 7.347880794884120722E-16, 4.500000000000000888 ) ) ;
#8448 = AXIS2_PLACEMENT_3D ( 'NONE', #4693, #2452, #12881 ) ;
#8449 = CIRCLE ( 'NONE', #5292, 3.799999999999999378 ) ;
#8451 = AXIS2_PLACEMENT_3D ( 'NONE', #13352, #13278, #13436 ) ;
#8450 = CARTESIAN_POINT ( 'NONE',  ( 2.697960371751379149, 11.73065272960063155, 9.756102650610282367 ) ) ;
#8452 = VERTEX_POINT ( 'NONE', #10520 ) ;
#8453 = CARTESIAN_POINT ( 'NONE',  ( 1.394999999999999574, 27.76164181293051669, 4.147968289691385202 ) ) ;
#8454 = CIRCLE ( 'NONE', #5780, 4.424999999999999822 ) ;
#8455 = AXIS2_PLACEMENT_3D ( 'NONE', #8316, #14160, #9616 ) ;
#8456 = VERTEX_POINT ( 'NONE', #1215 ) ;
#8457 = CARTESIAN_POINT ( 'NONE',  ( -14.40394475573012301, -4.794738323547945491, 20.00000000000000000 ) ) ;
#8458 = CARTESIAN_POINT ( 'NONE',  ( 0.7686372590627860157, -16.74220655292933913, -5.021526291670494579 ) ) ;
#8459 = ORIENTED_EDGE ( 'NONE', *, *, #545, .T. ) ;
#8460 = ORIENTED_EDGE ( 'NONE', *, *, #12351, .T. ) ;
#8461 = DIRECTION ( 'NONE',  ( 1.000000000000000000, 0.000000000000000000, 0.000000000000000000 ) ) ;
#8462 = VECTOR ( 'NONE', #13084, 1000.000000000000000 ) ;
#8463 = VERTEX_POINT ( 'NONE', #15219 ) ;
#8464 = AXIS2_PLACEMENT_3D ( 'NONE', #15178, #9248, #2182 ) ;
#8465 = AXIS2_PLACEMENT_3D ( 'NONE', #13492, #2963, #14876 ) ;
#8466 = FACE_OUTER_BOUND ( 'NONE', #5731, .T. ) ;
#8467 = CARTESIAN_POINT ( 'NONE',  ( 2.790000000000000480, -22.37986894186679265, 9.514945144208653005 ) ) ;
#8468 = CARTESIAN_POINT ( 'NONE',  ( 0.1882239034349760531, 12.84621645676876867, -22.54313264454999199 ) ) ;
#8469 = CARTESIAN_POINT ( 'NONE',  ( 2.604434261026090880, -25.39738473784997552, -5.253342437939998888 ) ) ;
#8470 = ORIENTED_EDGE ( 'NONE', *, *, #6661, .T. ) ;
#8471 = LINE ( 'NONE', #7256, #3503 ) ;
#8472 = EDGE_CURVE ( 'NONE', #1779, #12872, #3397, .T. ) ;
#8473 = CARTESIAN_POINT ( 'NONE',  ( 2.765633920072235519, -18.55949924794880346, -16.37294372382878649 ) ) ;
#8474 = ORIENTED_EDGE ( 'NONE', *, *, #6381, .T. ) ;
#8475 = DIRECTION ( 'NONE',  ( 0.000000000000000000, 0.000000000000000000, 1.000000000000000000 ) ) ;
#8476 = AXIS2_PLACEMENT_3D ( 'NONE', #14780, #11236, #624 ) ;
#8477 = ORIENTED_EDGE ( 'NONE', *, *, #264, .F. ) ;
#8478 = ORIENTED_EDGE ( 'NONE', *, *, #2575, .F. ) ;
#8479 = CARTESIAN_POINT ( 'NONE',  ( 2.789999999999999147, 8.624777288397799779, 11.04103753892274753 ) ) ;
#8480 = CARTESIAN_POINT ( 'NONE',  ( 0.000000000000000000, -24.34211360614294506, -7.909232158575071558 ) ) ;
#8481 = CARTESIAN_POINT ( 'NONE',  ( 1.749999999999998002, -25.12109765559643648, -12.52377138324252570 ) ) ;
#8482 = CARTESIAN_POINT ( 'NONE',  ( 2.789999999999999147, 13.40591150984237245, -7.739906618939567551 ) ) ;
#8483 = CARTESIAN_POINT ( 'NONE',  ( 33.82574562093736859, -6.697933970950280091, -2.000000000000000888 ) ) ;
#8484 = ADVANCED_FACE ( 'NONE', ( #12013 ), #1496, .T. ) ;
#8485 = CIRCLE ( 'NONE', #12670, 2.999999999999988898 ) ;
#8486 = CARTESIAN_POINT ( 'NONE',  ( 2.790000000000000036, 18.34424029220134500, -15.96500990068104997 ) ) ;
#8487 = AXIS2_PLACEMENT_3D ( 'NONE', #13666, #9073, #5166 ) ;
#8488 = EDGE_CURVE ( 'NONE', #15084, #1974, #14389, .T. ) ;
#8489 = ORIENTED_EDGE ( 'NONE', *, *, #11899, .T. ) ;
#8490 = CARTESIAN_POINT ( 'NONE',  ( 18.40394475573011945, -10.79473832354794460, 6.000000000000000000 ) ) ;
#8491 = DIRECTION ( 'NONE',  ( 1.000000000000000000, 0.000000000000000000, 0.000000000000000000 ) ) ;
#8492 = CARTESIAN_POINT ( 'NONE',  ( 0.4472135954999577612, 0.000000000000000000, 5.400000000000000355 ) ) ;
#8493 = PLANE ( 'NONE',  #13921 ) ;
#8494 = ORIENTED_EDGE ( 'NONE', *, *, #4796, .F. ) ;
#8495 = EDGE_CURVE ( 'NONE', #14323, #6652, #6257, .T. ) ;
#8496 = B_SPLINE_CURVE_WITH_KNOTS ( 'NONE', 3,
 ( #1372, #4702, #1295, #11753 ),
 .UNSPECIFIED., .F., .F.,
 ( 4, 4 ),
 ( 0.003263275852154239043, 0.003756984793529996591 ),
 .UNSPECIFIED. ) ;
#8497 = ORIENTED_EDGE ( 'NONE', *, *, #11881, .T. ) ;
#8498 = AXIS2_PLACEMENT_3D ( 'NONE', #11987, #1473, #5869 ) ;
#8499 = ORIENTED_EDGE ( 'NONE', *, *, #8533, .F. ) ;
#8500 = CIRCLE ( 'NONE', #1888, 17.95481323787947758 ) ;
#8501 = LINE ( 'NONE', #11188, #10008 ) ;
#8502 = AXIS2_PLACEMENT_3D ( 'NONE', #2013, #7777, #6699 ) ;
#8503 = CARTESIAN_POINT ( 'NONE',  ( 1.039999999999997593, 0.000000000000000000, 0.000000000000000000 ) ) ;
#8504 = CIRCLE ( 'NONE', #655, 2.524999999999996358 ) ;
#8505 = CYLINDRICAL_SURFACE ( 'NONE', #13621, 13.19999999999999929 ) ;
#8506 = DIRECTION ( 'NONE',  ( -0.9021244663126475327, 0.4314758942051350465, 9.480662228539550406E-17 ) ) ;
#8507 = CARTESIAN_POINT ( 'NONE',  ( 2.789999999999999147, -7.739906618939614624, -13.40591150984234581 ) ) ;
#8508 = EDGE_CURVE ( 'NONE', #7883, #12602, #14723, .T. ) ;
#8509 = ORIENTED_EDGE ( 'NONE', *, *, #9250, .T. ) ;
#8510 = CARTESIAN_POINT ( 'NONE',  ( 2.646101151981377075, 14.59528211759998406, 5.279841123860917307 ) ) ;
#8511 = CARTESIAN_POINT ( 'NONE',  ( 2.765633920072233742, -24.15498966839966855, 5.391175441198523544 ) ) ;
#8512 = EDGE_LOOP ( 'NONE', ( #3584, #5304, #5987, #13169 ) ) ;
#8514 = AXIS2_PLACEMENT_3D ( 'NONE', #1508, #8646, #13332 ) ;
#8513 = FACE_OUTER_BOUND ( 'NONE', #8000, .T. ) ;
#8515 = CARTESIAN_POINT ( 'NONE',  ( -14.40394475573012301, -4.794738323547945491, 16.99999999999999645 ) ) ;
#8516 = CARTESIAN_POINT ( 'NONE',  ( 80.00000000000000000, 0.000000000000000000, 6.000000000000000000 ) ) ;
#8517 = VERTEX_POINT ( 'NONE', #13552 ) ;
#8518 = EDGE_CURVE ( 'NONE', #13761, #10809, #7492, .T. ) ;
#8519 = CIRCLE ( 'NONE', #6803, 2.524999999999997247 ) ;
#8520 = CARTESIAN_POINT ( 'NONE',  ( 0.000000000000000000, 2.680914349914567470E-13, -23.06981291497571362 ) ) ;
#8522 = VECTOR ( 'NONE', #10359, 1000.000000000000000 ) ;
#8521 = FACE_OUTER_BOUND ( 'NONE', #4199, .T. ) ;
#8523 = ORIENTED_EDGE ( 'NONE', *, *, #14307, .F. ) ;
#8524 = ORIENTED_EDGE ( 'NONE', *, *, #14171, .T. ) ;
#8525 = EDGE_LOOP ( 'NONE', ( #15072, #5663, #5512, #4423, #5856 ) ) ;
#8526 = CARTESIAN_POINT ( 'NONE',  ( 0.000000000000000000, 20.62201879784911540, 12.52067188844362100 ) ) ;
#8527 = ADVANCED_FACE ( 'NONE', ( #13397 ), #14565, .T. ) ;
#8528 = PLANE ( 'NONE',  #707 ) ;
#8529 = CARTESIAN_POINT ( 'NONE',  ( 1.039999999999996483, 17.39253030560841395, 4.458161950358563885 ) ) ;
#8530 = CARTESIAN_POINT ( 'NONE',  ( 2.021362756903525959, -4.022333916463714409, 17.00993931356759603 ) ) ;
#8531 = FACE_OUTER_BOUND ( 'NONE', #10450, .T. ) ;
#8532 = EDGE_CURVE ( 'NONE', #2696, #7479, #10025, .T. ) ;
#8533 = EDGE_CURVE ( 'NONE', #8659, #797, #2816, .T. ) ;
#8534 = AXIS2_PLACEMENT_3D ( 'NONE', #2733, #14257, #1424 ) ;
#8535 = CARTESIAN_POINT ( 'NONE',  ( 33.82574562093736859, -6.697933970950280091, 2.999999999999999112 ) ) ;
#8536 = VERTEX_POINT ( 'NONE', #12250 ) ;
#8537 = AXIS2_PLACEMENT_3D ( 'NONE', #12660, #9214, #6905 ) ;
#8538 = CARTESIAN_POINT ( 'NONE',  ( 80.00000000000000000, -9.999999999999994671, 6.000000000000000000 ) ) ;
#8539 = VECTOR ( 'NONE', #2091, 1000.000000000000000 ) ;
#8540 = B_SPLINE_CURVE_WITH_KNOTS ( 'NONE', 3,
 ( #8618, #2940, #7627, #12378 ),
 .UNSPECIFIED., .F., .F.,
 ( 4, 4 ),
 ( 0.005123713096549405849, 0.005814346476695844007 ),
 .UNSPECIFIED. ) ;
#8541 =( LENGTH_UNIT ( ) NAMED_UNIT ( * ) SI_UNIT ( .MILLI., .METRE. ) );
#8542 = EDGE_LOOP ( 'NONE', ( #11023, #4715, #4853, #3666 ) ) ;
#8543 = ORIENTED_EDGE ( 'NONE', *, *, #3705, .F. ) ;
#8544 = DIRECTION ( 'NONE',  ( -1.000000000000000000, -0.000000000000000000, -0.000000000000000000 ) ) ;
#8545 = FACE_OUTER_BOUND ( 'NONE', #7280, .T. ) ;
#8546 = EDGE_LOOP ( 'NONE', ( #9508, #12319, #8332, #4753, #11475, #3994, #2626, #10002 ) ) ;
#8547 = AXIS2_PLACEMENT_3D ( 'NONE', #9955, #10874, #4043 ) ;
#8548 = EDGE_CURVE ( 'NONE', #6540, #10385, #14791, .T. ) ;
#8549 = ORIENTED_EDGE ( 'NONE', *, *, #227, .T. ) ;
#8550 = DIRECTION ( 'NONE',  ( -0.000000000000000000, -0.000000000000000000, 1.000000000000000000 ) ) ;
#8551 = CARTESIAN_POINT ( 'NONE',  ( 0.02436607992775934733, -2.336989772644440855, 24.63872515616082026 ) ) ;
#8552 = EDGE_CURVE ( 'NONE', #4548, #3235, #6409, .T. ) ;
#8553 = CARTESIAN_POINT ( 'NONE',  ( 0.07181525480391388883, 12.74223776959231991, -21.92234060054331479 ) ) ;
#8554 = VERTEX_POINT ( 'NONE', #11093 ) ;
#8555 = VECTOR ( 'NONE', #5846, 1000.000000000000000 ) ;
#8556 = VECTOR ( 'NONE', #5946, 1000.000000000000000 ) ;
#8557 = DIRECTION ( 'NONE',  ( 0.02857142857142857054, -0.9995917534020515305, 0.000000000000000000 ) ) ;
#8558 = B_SPLINE_CURVE_WITH_KNOTS ( 'NONE', 3,
 ( #8396, #9563, #15132, #12012 ),
 .UNSPECIFIED., .F., .F.,
 ( 4, 4 ),
 ( 0.005258120783916810613, 0.005948386350302961936 ),
 .UNSPECIFIED. ) ;
#8559 = CARTESIAN_POINT ( 'NONE',  ( 2.790000000000079527, -18.34439787333494820, -15.96555658743782580 ) ) ;
#8560 = EDGE_LOOP ( 'NONE', ( #11746, #9943, #10702, #3646 ) ) ;
#8561 = CARTESIAN_POINT ( 'NONE',  ( 0.4522159468065707899, 12.42068120944081322, 11.13074453164208144 ) ) ;
#8562 = CARTESIAN_POINT ( 'NONE',  ( 2.715264182578264407, -14.31752701692933272, -5.299647274067250891 ) ) ;
#8563 = VERTEX_POINT ( 'NONE', #554 ) ;
#8564 = ORIENTED_EDGE ( 'NONE', *, *, #1586, .T. ) ;
#8565 = CARTESIAN_POINT ( 'NONE',  ( 2.782650442329439588, 9.045126717605779021, 11.23191127083866725 ) ) ;
#8566 = CARTESIAN_POINT ( 'NONE',  ( 2.789999999999999147, 2.336989772644613161, -24.63872515616080250 ) ) ;
#8567 =( NAMED_UNIT ( * ) SI_UNIT ( $, .STERADIAN. ) SOLID_ANGLE_UNIT ( ) );
#8568 = CARTESIAN_POINT ( 'NONE',  ( 0.1882239080259275332, 25.40949241676353410, 5.251266773802457877 ) ) ;
#8569 = VECTOR ( 'NONE', #14816, 1000.000000000000000 ) ;
#8570 = EDGE_CURVE ( 'NONE', #15052, #13028, #14866, .T. ) ;
#8571 = CYLINDRICAL_SURFACE ( 'NONE', #7123, 2.999999999999975131 ) ;
#8572 = EDGE_LOOP ( 'NONE', ( #5089, #9102, #7560, #12632 ) ) ;
#8573 = FACE_OUTER_BOUND ( 'NONE', #6083, .T. ) ;
#8574 = CARTESIAN_POINT ( 'NONE',  ( -20.63749999999999929, 0.000000000000000000, 0.000000000000000000 ) ) ;
#8575 = DIRECTION ( 'NONE',  ( 0.000000000000000000, 0.8090169943749527803, -0.5877852522924655876 ) ) ;
#8576 = FILL_AREA_STYLE ('',( #9959 ) ) ;
#8577 = ORIENTED_EDGE ( 'NONE', *, *, #15118, .T. ) ;
#8578 = VECTOR ( 'NONE', #1771, 1000.000000000000114 ) ;
#8579 = VERTEX_POINT ( 'NONE', #5272 ) ;
#8580 = EDGE_CURVE ( 'NONE', #1432, #3477, #992, .T. ) ;
#8581 = ORIENTED_EDGE ( 'NONE', *, *, #7899, .T. ) ;
#8582 = CYLINDRICAL_SURFACE ( 'NONE', #13930, 4.000000000000000000 ) ;
#8583 = CARTESIAN_POINT ( 'NONE',  ( 8.000000000000000000, 0.000000000000000000, 0.000000000000000000 ) ) ;
#8584 = EDGE_CURVE ( 'NONE', #5623, #159, #1878, .T. ) ;
#8585 = DIRECTION ( 'NONE',  ( -0.000000000000000000, -0.000000000000000000, -1.000000000000000000 ) ) ;
#8586 = CARTESIAN_POINT ( 'NONE',  ( 2.030753602223783094, -4.828194074574165384, -27.14986936243579763 ) ) ;
#8587 = DIRECTION ( 'NONE',  ( 1.000000000000000000, 0.000000000000000000, 0.000000000000000000 ) ) ;
#8588 = CYLINDRICAL_SURFACE ( 'NONE', #3997, 2.524999999999999467 ) ;
#8589 = VERTEX_POINT ( 'NONE', #10171 ) ;
#8590 = DIRECTION ( 'NONE',  ( -0.000000000000000000, -0.000000000000000000, -1.000000000000000000 ) ) ;
#8591 = CARTESIAN_POINT ( 'NONE',  ( 2.782672435525939125, 11.23174270417329268, 9.044896821682240073 ) ) ;
#8592 = CIRCLE ( 'NONE', #14500, 0.1000000000000002554 ) ;
#8593 = ORIENTED_EDGE ( 'NONE', *, *, #14613, .T. ) ;
#8594 = DIRECTION ( 'NONE',  ( -1.000000000000000000, 0.000000000000000000, 0.000000000000000000 ) ) ;
#8595 = CYLINDRICAL_SURFACE ( 'NONE', #4334, 17.95481323787947403 ) ;
#8596 = LINE ( 'NONE', #5080, #8257 ) ;
#8597 = ORIENTED_EDGE ( 'NONE', *, *, #5262, .T. ) ;
#8598 = B_SPLINE_CURVE_WITH_KNOTS ( 'NONE', 3,
 ( #7660, #11187, #663, #11852, #5815, #7185 ),
 .UNSPECIFIED., .F., .F.,
 ( 4, 2, 4 ),
 ( 4.462636808949230078E-07, 0.001879885123572232067, 0.003759323983463569441 ),
 .UNSPECIFIED. ) ;
#8599 = DIRECTION ( 'NONE',  ( -1.000000000000000000, -0.000000000000000000, 0.000000000000000000 ) ) ;
#8600 = CYLINDRICAL_SURFACE ( 'NONE', #6284, 2.524999999999999467 ) ;
#8601 = VERTEX_POINT ( 'NONE', #4338 ) ;
#8602 = EDGE_LOOP ( 'NONE', ( #2952, #5564, #8113, #2314 ) ) ;
#8603 = VERTEX_POINT ( 'NONE', #11248 ) ;
#8604 = CARTESIAN_POINT ( 'NONE',  ( 2.783068945535915439, 24.42321038836782776, -2.248820353273055517 ) ) ;
#8605 = CARTESIAN_POINT ( 'NONE',  ( 1.394999999999999574, -17.29145405592692342, 4.835383649608410828 ) ) ;
#8606 = CARTESIAN_POINT ( 'NONE',  ( 1.394999999999999574, -12.52377138324241734, 25.12109765559649688 ) ) ;
#8607 = CARTESIAN_POINT ( 'NONE',  ( 1.039999999999997371, -4.147968289691092991, -27.76164181293055933 ) ) ;
#8608 = DIRECTION ( 'NONE',  ( -1.000000000000000000, -0.000000000000000000, -0.000000000000000000 ) ) ;
#8609 = EDGE_CURVE ( 'NONE', #1278, #9070, #9022, .T. ) ;
#8610 = DIRECTION ( 'NONE',  ( -0.000000000000000000, -0.000000000000000000, 1.000000000000000000 ) ) ;
#8611 = VERTEX_POINT ( 'NONE', #4261 ) ;
#8612 = CARTESIAN_POINT ( 'NONE',  ( 80.82762530298222714, -9.999999999999994671, 4.000000000000003553 ) ) ;
#8613 = EDGE_CURVE ( 'NONE', #10328, #12415, #5545, .T. ) ;
#8614 = EDGE_CURVE ( 'NONE', #3527, #4006, #9054, .T. ) ;
#8615 = EDGE_CURVE ( 'NONE', #9774, #3458, #5763, .T. ) ;
#8616 = VERTEX_POINT ( 'NONE', #7939 ) ;
#8617 = ORIENTED_EDGE ( 'NONE', *, *, #6168, .T. ) ;
#8618 = CARTESIAN_POINT ( 'NONE',  ( 2.789999999999999147, -13.87420763704362514, 1.948757464274123885 ) ) ;
#8619 = LINE ( 'NONE', #7556, #8221 ) ;
#8620 = EDGE_LOOP ( 'NONE', ( #13549, #9455, #3033, #12752, #215, #2910, #8951, #12596 ) ) ;
#8621 = LINE ( 'NONE', #7632, #881 ) ;
#8622 = VERTEX_POINT ( 'NONE', #5718 ) ;
#8623 = CARTESIAN_POINT ( 'NONE',  ( 2.718184767880469810, -10.24584646439555691, 23.19431517146929878 ) ) ;
#8624 = CARTESIAN_POINT ( 'NONE',  ( 0.000000000000000000, 0.000000000000000000, 4.500000000000000888 ) ) ;
#8625 = EDGE_CURVE ( 'NONE', #3664, #2195, #8163, .T. ) ;
#8626 = EDGE_CURVE ( 'NONE', #11392, #3403, #7989, .T. ) ;
#8627 = CARTESIAN_POINT ( 'NONE',  ( 91.46153288930040048, 16.46030115554384565, -2.000000000000000888 ) ) ;
#8628 = DIRECTION ( 'NONE',  ( 0.000000000000000000, 0.000000000000000000, 1.000000000000000000 ) ) ;
#8629 = EDGE_CURVE ( 'NONE', #12163, #613, #1353, .T. ) ;
#8630 = DIRECTION ( 'NONE',  ( -1.000000000000000000, -0.000000000000000000, -0.000000000000000000 ) ) ;
#8631 = ORIENTED_EDGE ( 'NONE', *, *, #1488, .T. ) ;
#8632 = CARTESIAN_POINT ( 'NONE',  ( 1.039999999999996483, 17.29145405592695539, -4.835383649608292700 ) ) ;
#8633 = DIRECTION ( 'NONE',  ( -0.4571871344001417481, -0.8893705212896291235, 0.000000000000000000 ) ) ;
#8634 = ORIENTED_EDGE ( 'NONE', *, *, #460, .F. ) ;
#8635 = VERTEX_POINT ( 'NONE', #1175 ) ;
#8636 = CARTESIAN_POINT ( 'NONE',  ( 80.00000000000000000, 0.000000000000000000, 5.500000000000000000 ) ) ;
#8637 = DIRECTION ( 'NONE',  ( -1.000000000000000000, 0.000000000000000000, 0.000000000000000000 ) ) ;
#8638 = EDGE_CURVE ( 'NONE', #8452, #13251, #9788, .T. ) ;
#8639 = CIRCLE ( 'NONE', #2021, 17.95481323787947758 ) ;
#8640 = FACE_BOUND ( 'NONE', #123, .T. ) ;
#8641 = DIRECTION ( 'NONE',  ( 0.000000000000000000, 0.000000000000000000, 1.000000000000000000 ) ) ;
#8642 = ORIENTED_EDGE ( 'NONE', *, *, #3647, .T. ) ;
#8643 = DIRECTION ( 'NONE',  ( -0.9148936170212765839, -0.4036950204470272086, 0.000000000000000000 ) ) ;
#8644 = DIRECTION ( 'NONE',  ( 0.000000000000000000, 0.000000000000000000, -1.000000000000000000 ) ) ;
#8645 = FACE_OUTER_BOUND ( 'NONE', #5293, .T. ) ;
#8646 = DIRECTION ( 'NONE',  ( -1.000000000000000000, 0.000000000000000000, -0.000000000000000000 ) ) ;
#8647 = VECTOR ( 'NONE', #11516, 1000.000000000000000 ) ;
#8648 = ORIENTED_EDGE ( 'NONE', *, *, #8303, .T. ) ;
#8649 = ORIENTED_EDGE ( 'NONE', *, *, #6275, .T. ) ;
#8650 = ORIENTED_EDGE ( 'NONE', *, *, #660, .T. ) ;
#8651 = DIRECTION ( 'NONE',  ( 0.000000000000000000, 0.000000000000000000, 1.000000000000000000 ) ) ;
#8652 = CARTESIAN_POINT ( 'NONE',  ( 101.6227766016837819, -9.999999999999994671, 3.000000000000002665 ) ) ;
#8653 = CARTESIAN_POINT ( 'NONE',  ( 2.601776144743014996, -23.64332819722373813, -10.68696068830432466 ) ) ;
#8654 = CARTESIAN_POINT ( 'NONE',  ( -15.94493884710238696, -7.321218896460230496, -3.000000000000000000 ) ) ;
#8655 = SHAPE_DEFINITION_REPRESENTATION ( #2954, #7891 ) ;
#8656 = CARTESIAN_POINT ( 'NONE',  ( 80.00000000000000000, 0.000000000000000000, 4.000000000000003553 ) ) ;
#8657 = CARTESIAN_POINT ( 'NONE',  ( 2.789999999999999147, -0.2301004812059262439, 24.44424927289185590 ) ) ;
#8658 = CARTESIAN_POINT ( 'NONE',  ( 0.02436607992776368414, 18.55949924794916228, -16.37294372382838148 ) ) ;
#8659 = VERTEX_POINT ( 'NONE', #10327 ) ;
#8660 = DIRECTION ( 'NONE',  ( 0.000000000000000000, 0.000000000000000000, -1.000000000000000000 ) ) ;
#8661 = CARTESIAN_POINT ( 'NONE',  ( 67.23404255319145761, 28.93147646537026318, 4.000000000000003553 ) ) ;
#8662 = ORIENTED_EDGE ( 'NONE', *, *, #10774, .F. ) ;
#8663 = CARTESIAN_POINT ( 'NONE',  ( 0.000000000000000000, -8.624777288397881492, 11.04103753892268891 ) ) ;
#8664 = CARTESIAN_POINT ( 'NONE',  ( 0.04999671152047703571, -14.75565684666127986, 2.439987328296917557 ) ) ;
#8665 = ORIENTED_EDGE ( 'NONE', *, *, #7289, .T. ) ;
#8666 = EDGE_LOOP ( 'NONE', ( #3586, #341, #6741, #6010, #13227, #8939, #7728, #496, #3126, #11228, #6818, #7420, #13682, #11620, #2074, #419, #11508, #5425, #11672, #4339, #5215, #13942, #3920, #10995, #13589, #2251, #1216 ) ) ;
#8667 = CARTESIAN_POINT ( 'NONE',  ( 2.789999999999999147, 15.74360496233408213, -18.28042085475260592 ) ) ;
#8668 = DIRECTION ( 'NONE',  ( 1.000000000000000000, -0.000000000000000000, -0.000000000000000000 ) ) ;
#8669 = CARTESIAN_POINT ( 'NONE',  ( 0.02531912748631468327, -14.46287784598615644, -2.311161484776706576 ) ) ;
#8670 = CARTESIAN_POINT ( 'NONE',  ( 0.007327532539345395050, -2.217238903388463189, -14.24942254254691854 ) ) ;
#8671 = PRODUCT_DEFINITION_FORMATION_WITH_SPECIFIED_SOURCE ( 'ANY', '', #2824, .NOT_KNOWN. ) ;
#8672 = DIRECTION ( 'NONE',  ( -1.445602896647338917E-16, 1.000000000000000000, -0.000000000000000000 ) ) ;
#8673 = ORIENTED_EDGE ( 'NONE', *, *, #3647, .F. ) ;
#8674 = DIRECTION ( 'NONE',  ( 0.8894282943767740646, 0.4570747303910190351, -9.680251508487129501E-17 ) ) ;
#8675 = EDGE_CURVE ( 'NONE', #7151, #10675, #4065, .T. ) ;
#8676 = AXIS2_PLACEMENT_3D ( 'NONE', #5881, #12000, #6019 ) ;
#8677 = ADVANCED_FACE ( 'NONE', ( #15021 ), #1024, .T. ) ;
#8678 = ORIENTED_EDGE ( 'NONE', *, *, #47, .F. ) ;
#8679 = ORIENTED_EDGE ( 'NONE', *, *, #9619, .F. ) ;
#8680 = EDGE_LOOP ( 'NONE', ( #13537, #12730, #7608, #8649 ) ) ;
#8681 = CYLINDRICAL_SURFACE ( 'NONE', #13633, 2.447112362156698140 ) ;
#8682 = VECTOR ( 'NONE', #10215, 1000.000000000000000 ) ;
#8683 = SURFACE_STYLE_FILL_AREA ( #11002 ) ;
#8684 = VERTEX_POINT ( 'NONE', #12621 ) ;
#8685 = AXIS2_PLACEMENT_3D ( 'NONE', #14861, #632, #14785 ) ;
#8686 = AXIS2_PLACEMENT_3D ( 'NONE', #8108, #3419, #13001 ) ;
#8687 = PRODUCT_DEFINITION_CONTEXT ( 'detailed design', #5084, 'design' ) ;
#8688 = DIRECTION ( 'NONE',  ( -0.9237280213470681067, -0.3830490080632377725, 0.000000000000000000 ) ) ;
#8689 = EDGE_CURVE ( 'NONE', #13319, #447, #8098, .T. ) ;
#8690 = ORIENTED_EDGE ( 'NONE', *, *, #2708, .T. ) ;
#8691 = EDGE_CURVE ( 'NONE', #11975, #3303, #5652, .T. ) ;
#8692 = B_SPLINE_CURVE_WITH_KNOTS ( 'NONE', 3,
 ( #12230, #10005, #6546, #12145 ),
 .UNSPECIFIED., .F., .F.,
 ( 4, 4 ),
 ( 2.159563976726664397E-07, 0.0006916893629248962961 ),
 .UNSPECIFIED. ) ;
#8693 = CARTESIAN_POINT ( 'NONE',  ( 0.000000000000000000, 0.000000000000000000, 10.00000000000000000 ) ) ;
#8694 = CIRCLE ( 'NONE', #14608, 24.12539914357697413 ) ;
#8695 = AXIS2_PLACEMENT_3D ( 'NONE', #14634, #8852, #11240 ) ;
#8696 = CYLINDRICAL_SURFACE ( 'NONE', #1574, 2.524999999999995914 ) ;
#8697 = AXIS2_PLACEMENT_3D ( 'NONE', #10862, #13249, #2730 ) ;
#8698 = DIRECTION ( 'NONE',  ( 1.000000000000000000, 0.000000000000000000, 0.000000000000000000 ) ) ;
#8699 = CARTESIAN_POINT ( 'NONE',  ( 0.02531912748464674665, 11.36963888406700285, -9.232963481057645083 ) ) ;
#8700 = ORIENTED_EDGE ( 'NONE', *, *, #453, .F. ) ;
#8701 = DIRECTION ( 'NONE',  ( 0.9863939238321437486, 0.1643989873053574857, -0.000000000000000000 ) ) ;
#8702 = CARTESIAN_POINT ( 'NONE',  ( 2.789999999999999147, 11.36963888406687317, 9.232963481057801403 ) ) ;
#8703 = AXIS2_PLACEMENT_3D ( 'NONE', #5070, #6282, #6134 ) ;
#8704 = VERTEX_POINT ( 'NONE', #7874 ) ;
#8705 = VERTEX_POINT ( 'NONE', #869 ) ;
#8706 = CARTESIAN_POINT ( 'NONE',  ( -7.765813458258934317E-14, -24.22524813288764278, 2.133839912090720325 ) ) ;
#8708 = PLANE ( 'NONE',  #4141 ) ;
#8707 = AXIS2_PLACEMENT_3D ( 'NONE', #4878, #8168, #2327 ) ;
#8709 = EDGE_CURVE ( 'NONE', #3460, #3172, #4308, .T. ) ;
#8710 = CIRCLE ( 'NONE', #12394, 24.12539914357697768 ) ;
#8711 =( NAMED_UNIT ( * ) PLANE_ANGLE_UNIT ( ) SI_UNIT ( $, .RADIAN. ) );
#8712 = DIRECTION ( 'NONE',  ( 0.000000000000000000, 0.000000000000000000, 1.000000000000000000 ) ) ;
#8713 = EDGE_CURVE ( 'NONE', #11370, #6946, #1096, .T. ) ;
#8714 = ADVANCED_FACE ( 'NONE', ( #9101 ), #4720, .F. ) ;
#8715 = CARTESIAN_POINT ( 'NONE',  ( 14.40394475573011945, -10.79473832354794460, 5.500000000000001776 ) ) ;
#8716 = B_SPLINE_CURVE_WITH_KNOTS ( 'NONE', 3,
 ( #7671, #7381, #1454, #5002, #9977, #11053 ),
 .UNSPECIFIED., .F., .F.,
 ( 4, 2, 4 ),
 ( 4.462636677693390501E-07, 0.001879885020955137558, 0.003759323778242505774 ),
 .UNSPECIFIED. ) ;
#8717 = ORIENTED_EDGE ( 'NONE', *, *, #5625, .T. ) ;
#8718 = CARTESIAN_POINT ( 'NONE',  ( 2.789999999999999147, 0.000000000000000000, 0.000000000000000000 ) ) ;
#8719 = CARTESIAN_POINT ( 'NONE',  ( 0.006931069955678950678, -18.43696893154746164, -16.17493693894899209 ) ) ;
#8720 = AXIS2_PLACEMENT_3D ( 'NONE', #11008, #8778, #233 ) ;
#8721 = CARTESIAN_POINT ( 'NONE',  ( 2.789999999999999147, -18.28042085475289369, 15.74360496233375173 ) ) ;
#8722 = EDGE_CURVE ( 'NONE', #13244, #8579, #7501, .T. ) ;
#8723 = AXIS2_PLACEMENT_3D ( 'NONE', #6162, #8378, #6091 ) ;
#8724 = VERTEX_POINT ( 'NONE', #2097 ) ;
#8725 = ORIENTED_EDGE ( 'NONE', *, *, #8584, .T. ) ;
#8726 = VERTEX_POINT ( 'NONE', #5876 ) ;
#8727 = CARTESIAN_POINT ( 'NONE',  ( 1.749999999999998002, 25.12109765559653596, 12.52377138324232675 ) ) ;
#8728 = DIRECTION ( 'NONE',  ( 0.000000000000000000, 0.000000000000000000, 1.000000000000000000 ) ) ;
#8729 = CARTESIAN_POINT ( 'NONE',  ( 2.789999999999999147, -24.63872515616084513, 2.336989772644183283 ) ) ;
#8730 = CARTESIAN_POINT ( 'NONE',  ( 0.007349557670559583172, 11.23191127083863350, 9.045126717605816324 ) ) ;
#8731 = APPLICATION_PROTOCOL_DEFINITION ( 'draft international standard', 'automotive_design', 1998, #1833 ) ;
#8732 = DIRECTION ( 'NONE',  ( 1.000000000000000000, -0.000000000000000000, -0.000000000000000000 ) ) ;
#8733 = CIRCLE ( 'NONE', #9239, 4.000000000000000000 ) ;
#8734 = DIRECTION ( 'NONE',  ( 0.9148936170212768060, 0.4036950204470268200, -0.000000000000000000 ) ) ;
#8735 = LINE ( 'NONE', #13430, #13091 ) ;
#8736 = ORIENTED_EDGE ( 'NONE', *, *, #1873, .T. ) ;
#8737 = FACE_OUTER_BOUND ( 'NONE', #1788, .T. ) ;
#8738 = DIRECTION ( 'NONE',  ( 0.000000000000000000, 0.000000000000000000, -1.000000000000000000 ) ) ;
#8739 = FACE_OUTER_BOUND ( 'NONE', #13865, .T. ) ;
#8740 = EDGE_CURVE ( 'NONE', #9424, #7105, #6869, .T. ) ;
#8741 = ORIENTED_EDGE ( 'NONE', *, *, #9553, .F. ) ;
#8742 = AXIS2_PLACEMENT_3D ( 'NONE', #3067, #6750, #13665 ) ;
#8743 = CARTESIAN_POINT ( 'NONE',  ( 1.749999999999999778, 0.000000000000000000, 0.000000000000000000 ) ) ;
#8744 = CARTESIAN_POINT ( 'NONE',  ( 2.789999999999999147, 9.999777909380087593, -11.07980565117269833 ) ) ;
#8745 = ORIENTED_EDGE ( 'NONE', *, *, #9951, .T. ) ;
#8746 = COLOUR_RGB ( '',1.000000000000000000, 0.9490196078431372140, 0.9098039215686274384 ) ;
#8747 = CIRCLE ( 'NONE', #7285, 28.06981291497571007 ) ;
#8748 = EDGE_LOOP ( 'NONE', ( #3758, #7838, #6274, #9355, #11256, #14135 ) ) ;
#8749 = FACE_OUTER_BOUND ( 'NONE', #1079, .T. ) ;
#8750 = CARTESIAN_POINT ( 'NONE',  ( 72.68384697807672978, 11.35494834827056110, 4.000000000000000000 ) ) ;
#8751 = DIRECTION ( 'NONE',  ( -1.000000000000000000, -0.000000000000000000, -0.000000000000000000 ) ) ;
#8752 = DIRECTION ( 'NONE',  ( 0.000000000000000000, -0.000000000000000000, -1.000000000000000000 ) ) ;
#8753 = DIRECTION ( 'NONE',  ( -1.000000000000000000, 0.000000000000000000, 0.000000000000000000 ) ) ;
#8754 = EDGE_CURVE ( 'NONE', #10954, #13796, #3007, .T. ) ;
#8755 = PRESENTATION_LAYER_ASSIGNMENT (  '', '', ( #3118 ) ) ;
#8756 = LINE ( 'NONE', #2930, #8578 ) ;
#8757 = EDGE_CURVE ( 'NONE', #9373, #1519, #11175, .T. ) ;
#8758 = ORIENTED_EDGE ( 'NONE', *, *, #5121, .T. ) ;
#8759 = DIRECTION ( 'NONE',  ( 0.000000000000000000, 0.000000000000000000, 1.000000000000000000 ) ) ;
#8760 = CIRCLE ( 'NONE', #5825, 5.400000000000000355 ) ;
#8761 = AXIS2_PLACEMENT_3D ( 'NONE', #3670, #8133, #4919 ) ;
#8762 = UNCERTAINTY_MEASURE_WITH_UNIT (LENGTH_MEASURE( 1.000000000000000082E-05 ), #5206, 'distance_accuracy_value', 'NONE');
#8763 = DIRECTION ( 'NONE',  ( 0.000000000000000000, 0.000000000000000000, 1.000000000000000000 ) ) ;
#8764 = CIRCLE ( 'NONE', #2639, 0.5999999999999998668 ) ;
#8765 =( NAMED_UNIT ( * ) PLANE_ANGLE_UNIT ( ) SI_UNIT ( $, .RADIAN. ) );
#8766 = EDGE_LOOP ( 'NONE', ( #14875, #2672, #8021, #3773 ) ) ;
#8767 = ORIENTED_EDGE ( 'NONE', *, *, #11437, .T. ) ;
#8768 = ORIENTED_EDGE ( 'NONE', *, *, #3200, .T. ) ;
#8769 = DIRECTION ( 'NONE',  ( -1.000000000000000000, 0.000000000000000000, 0.000000000000000000 ) ) ;
#8770 = EDGE_CURVE ( 'NONE', #11997, #6540, #6018, .T. ) ;
#8771 = CARTESIAN_POINT ( 'NONE',  ( 2.257825477245773982, 18.57583492944447556, -19.66801664102683489 ) ) ;
#8772 = EDGE_LOOP ( 'NONE', ( #1920, #9954, #13502, #4842 ) ) ;
#8773 = AXIS2_PLACEMENT_3D ( 'NONE', #5593, #9045, #11411 ) ;
#8774 = AXIS2_PLACEMENT_3D ( 'NONE', #3428, #4816, #10725 ) ;
#8775 = EDGE_CURVE ( 'NONE', #368, #6042, #8710, .T. ) ;
#8776 = AXIS2_PLACEMENT_3D ( 'NONE', #7912, #6755, #11432 ) ;
#8777 = DIRECTION ( 'NONE',  ( -1.000000000000000000, -0.000000000000000000, -0.000000000000000000 ) ) ;
#8778 = DIRECTION ( 'NONE',  ( -0.000000000000000000, -0.000000000000000000, 1.000000000000000000 ) ) ;
#8779 = VERTEX_POINT ( 'NONE', #385 ) ;
#8780 = DIRECTION ( 'NONE',  ( 0.7573544145849105957, -0.6530040510661073716, -2.081668171172162967E-17 ) ) ;
#8781 = DIRECTION ( 'NONE',  ( 1.000000000000000000, 0.000000000000000000, 0.000000000000000000 ) ) ;
#8782 = DIRECTION ( 'NONE',  ( 1.000000000000000000, 0.000000000000000000, 0.000000000000000000 ) ) ;
#8783 = AXIS2_PLACEMENT_3D ( 'NONE', #7312, #7079, #5932 ) ;
#8784 = CARTESIAN_POINT ( 'NONE',  ( 2.789999999999999147, 20.70663861606293210, -12.51925356660738053 ) ) ;
#8785 = DIRECTION ( 'NONE',  ( 0.000000000000000000, 0.000000000000000000, 1.000000000000000000 ) ) ;
#8786 = AXIS2_PLACEMENT_3D ( 'NONE', #9344, #5816, #4590 ) ;
#8787 = ORIENTED_EDGE ( 'NONE', *, *, #7895, .T. ) ;
#8788 = DIRECTION ( 'NONE',  ( 0.02857142857142857054, 0.9995917534020515305, 0.000000000000000000 ) ) ;
#8789 = ADVANCED_FACE ( 'NONE', ( #1246 ), #12140, .T. ) ;
#8790 = DIRECTION ( 'NONE',  ( 0.000000000000000000, 0.000000000000000000, 1.000000000000000000 ) ) ;
#8791 = ORIENTED_EDGE ( 'NONE', *, *, #1840, .F. ) ;
#8792 = VERTEX_POINT ( 'NONE', #13147 ) ;
#8793 = CARTESIAN_POINT ( 'NONE',  ( 1.749999999999998002, 0.000000000000000000, 0.000000000000000000 ) ) ;
#8794 = DIRECTION ( 'NONE',  ( -0.000000000000000000, -0.000000000000000000, -1.000000000000000000 ) ) ;
#8795 = CARTESIAN_POINT ( 'NONE',  ( 2.604434261026087771, 25.39738473785002526, 5.253342437939815923 ) ) ;
#8796 = EDGE_CURVE ( 'NONE', #2082, #7850, #6092, .T. ) ;
#8797 = FACE_OUTER_BOUND ( 'NONE', #8766, .T. ) ;
#8798 = CIRCLE ( 'NONE', #6844, 4.000000000000000000 ) ;
#8799 = CIRCLE ( 'NONE', #2918, 4.000000000000000000 ) ;
#8800 = ORIENTED_EDGE ( 'NONE', *, *, #8120, .F. ) ;
#8801 = CARTESIAN_POINT ( 'NONE',  ( 2.765633920072235519, 9.836394144776026138, -22.71065055754441531 ) ) ;
#8802 = LINE ( 'NONE', #5370, #8158 ) ;
#8803 = ORIENTED_EDGE ( 'NONE', *, *, #14955, .F. ) ;
#8804 = ORIENTED_EDGE ( 'NONE', *, *, #5864, .F. ) ;
#8805 = ORIENTED_EDGE ( 'NONE', *, *, #11532, .T. ) ;
#8806 = ADVANCED_FACE ( 'NONE', ( #1480 ), #14395, .T. ) ;
#8807 = EDGE_CURVE ( 'NONE', #6626, #6827, #307, .T. ) ;
#8808 = VERTEX_POINT ( 'NONE', #12991 ) ;
#8809 =( REPRESENTATION_RELATIONSHIP ('NONE','NONE', #12685, #7891 ) REPRESENTATION_RELATIONSHIP_WITH_TRANSFORMATION ( #9723 )SHAPE_REPRESENTATION_RELATIONSHIP( ) );
#8810 = AXIS2_PLACEMENT_3D ( 'NONE', #6967, #11647, #3581 ) ;
#8811 = CARTESIAN_POINT ( 'NONE',  ( 3.948182771089140175, -23.68909662653485171, 2.000000000000000000 ) ) ;
#8812 = CIRCLE ( 'NONE', #12495, 4.000000000000000000 ) ;
#8813 = PLANE ( 'NONE',  #2891 ) ;
#8814 = DIRECTION ( 'NONE',  ( 0.4570747303910190351, -0.8894282943767740646, 6.847307257068341160E-17 ) ) ;
#8815 = FACE_OUTER_BOUND ( 'NONE', #4606, .T. ) ;
#8816 = PLANE ( 'NONE',  #11752 ) ;
#8817 = DIRECTION ( 'NONE',  ( 0.7573544145849105957, -0.6530040510661073716, -2.081668171172162967E-17 ) ) ;
#8818 = ORIENTED_EDGE ( 'NONE', *, *, #9923, .T. ) ;
#8819 = LINE ( 'NONE', #1453, #2903 ) ;
#8820 = CARTESIAN_POINT ( 'NONE',  ( -1.150000000000001688, 0.000000000000000000, -6.000000000000001776 ) ) ;
#8821 = EDGE_CURVE ( 'NONE', #11883, #6223, #14314, .T. ) ;
#8822 = CARTESIAN_POINT ( 'NONE',  ( 80.00000000000000000, 0.000000000000000000, 4.000000000000003553 ) ) ;
#8823 = ADVANCED_FACE ( 'NONE', ( #8545, #6235 ), #7403, .F. ) ;
#8824 = ORIENTED_EDGE ( 'NONE', *, *, #11205, .T. ) ;
#8825 = EDGE_CURVE ( 'NONE', #7330, #9808, #13120, .T. ) ;
#8826 = CARTESIAN_POINT ( 'NONE',  ( 1.039999999999996039, -12.83329210556840394, 12.55714665599982816 ) ) ;
#8827 = DIRECTION ( 'NONE',  ( 1.000000000000000000, 0.000000000000000000, 0.000000000000000000 ) ) ;
#8828 = VERTEX_POINT ( 'NONE', #3863 ) ;
#8829 = ORIENTED_EDGE ( 'NONE', *, *, #5263, .T. ) ;
#8830 = CARTESIAN_POINT ( 'NONE',  ( -5.209999999999999964, 0.000000000000000000, 0.000000000000000000 ) ) ;
#8831 = CARTESIAN_POINT ( 'NONE',  ( 62.65957446808508280, 26.91300136313512681, 7.000000000000000000 ) ) ;
#8832 = CARTESIAN_POINT ( 'NONE',  ( 2.764680872515352661, 9.232963481057920418, -11.36963888406677725 ) ) ;
#8833 = CARTESIAN_POINT ( 'NONE',  ( 2.789999999999999147, 24.34211360614310848, -7.909232158574561744 ) ) ;
#8834 = AXIS2_PLACEMENT_3D ( 'NONE', #12275, #3824, #14284 ) ;
#8835 = DIRECTION ( 'NONE',  ( 1.000000000000000000, 0.000000000000000000, 0.000000000000000000 ) ) ;
#8836 = EDGE_CURVE ( 'NONE', #3473, #1249, #12727, .T. ) ;
#8837 = DIRECTION ( 'NONE',  ( -1.000000000000000000, 0.000000000000000000, 0.000000000000000000 ) ) ;
#8838 = ORIENTED_EDGE ( 'NONE', *, *, #2512, .T. ) ;
#8839 = CARTESIAN_POINT ( 'NONE',  ( 2.789999999999999147, 0.000000000000000000, 0.000000000000000000 ) ) ;
#8840 = DIRECTION ( 'NONE',  ( 0.000000000000000000, 0.000000000000000000, -1.000000000000000000 ) ) ;
#8841 = ORIENTED_EDGE ( 'NONE', *, *, #711, .F. ) ;
#8842 = FILL_AREA_STYLE_COLOUR ( '', #14152 ) ;
#8843 = ORIENTED_EDGE ( 'NONE', *, *, #5331, .T. ) ;
#8844 = ORIENTED_EDGE ( 'NONE', *, *, #6921, .T. ) ;
#8845 = ORIENTED_EDGE ( 'NONE', *, *, #2301, .T. ) ;
#8846 = CARTESIAN_POINT ( 'NONE',  ( 4.000000000000000000, 4.898587196589412829E-16, 1.395000000000000462 ) ) ;
#8847 = CARTESIAN_POINT ( 'NONE',  ( 2.789895169984651702, -20.67846228565646172, -12.51925356660783528 ) ) ;
#8848 = UNCERTAINTY_MEASURE_WITH_UNIT (LENGTH_MEASURE( 1.000000000000000082E-05 ), #1546, 'distance_accuracy_value', 'NONE');
#8849 = CARTESIAN_POINT ( 'NONE',  ( -10.40394475573011945, -10.79473832354794460, -5.000000000000000000 ) ) ;
#8850 = LINE ( 'NONE', #13543, #1866 ) ;
#8851 = ORIENTED_EDGE ( 'NONE', *, *, #6938, .T. ) ;
#8852 = DIRECTION ( 'NONE',  ( 1.000000000000000000, 0.000000000000000000, 0.000000000000000000 ) ) ;
#8853 = CYLINDRICAL_SURFACE ( 'NONE', #1921, 10.00000000000000000 ) ;
#8854 = DIRECTION ( 'NONE',  ( -5.339417856040273846E-17, -1.063174570779084847E-17, 1.000000000000000000 ) ) ;
#8855 = CARTESIAN_POINT ( 'NONE',  ( 0.02436607992776281678, 2.336989772644269436, 24.63872515616083447 ) ) ;
#8856 = ADVANCED_FACE ( 'NONE', ( #13059 ), #2547, .T. ) ;
#8857 = ORIENTED_EDGE ( 'NONE', *, *, #2242, .T. ) ;
#8858 = FACE_OUTER_BOUND ( 'NONE', #7073, .T. ) ;
#8859 = CARTESIAN_POINT ( 'NONE',  ( 70.16198417812034904, 9.730076655429538590, 2.999999999999999112 ) ) ;
#8860 = ORIENTED_EDGE ( 'NONE', *, *, #4240, .T. ) ;
#8861 = VERTEX_POINT ( 'NONE', #10921 ) ;
#8862 = CARTESIAN_POINT ( 'NONE',  ( 2.789999999999999147, 14.59528211759997696, 3.120158876139284665 ) ) ;
#8863 = SURFACE_STYLE_FILL_AREA ( #11324 ) ;
#8864 = CARTESIAN_POINT ( 'NONE',  ( 98.63205416320636232, -2.094184955359750244, 3.000000000000000000 ) ) ;
#8865 = AXIS2_PLACEMENT_3D ( 'NONE', #12156, #479, #8557 ) ;
#8866 = ORIENTED_EDGE ( 'NONE', *, *, #6558, .F. ) ;
#8867 = CARTESIAN_POINT ( 'NONE',  ( 31.51081190520435626, 3.030430839836910639, 2.999999999999999112 ) ) ;
#8868 = ORIENTED_EDGE ( 'NONE', *, *, #2424, .F. ) ;
#8869 = CARTESIAN_POINT ( 'NONE',  ( 1.749999999999998002, 0.000000000000000000, 0.000000000000000000 ) ) ;
#8870 = DIRECTION ( 'NONE',  ( 1.000000000000000000, 0.000000000000000000, 0.000000000000000000 ) ) ;
#8871 = ORIENTED_EDGE ( 'NONE', *, *, #11076, .F. ) ;
#8872 = CARTESIAN_POINT ( 'NONE',  ( 58.14665764790533586, -0.9105996816177489572, 2.999999999999999112 ) ) ;
#8873 = EDGE_CURVE ( 'NONE', #13815, #9813, #5954, .T. ) ;
#8874 = DIRECTION ( 'NONE',  ( 0.000000000000000000, 0.000000000000000000, -1.000000000000000000 ) ) ;
#8875 = ORIENTED_EDGE ( 'NONE', *, *, #7853, .T. ) ;
#8876 = ORIENTED_EDGE ( 'NONE', *, *, #12295, .F. ) ;
#8877 = CIRCLE ( 'NONE', #15028, 7.000000000000000000 ) ;
#8878 = ADVANCED_FACE ( 'NONE', ( #8380 ), #7091, .T. ) ;
#8879 = ORIENTED_EDGE ( 'NONE', *, *, #3364, .F. ) ;
#8880 = CARTESIAN_POINT ( 'NONE',  ( 1.394999999999998685, 17.29145405592695894, -4.835383649608291812 ) ) ;
#8881 = CARTESIAN_POINT ( 'NONE',  ( 0.02436607992776585255, -5.391175441198789109, 24.15498966839961170 ) ) ;
#8882 = CARTESIAN_POINT ( 'NONE',  ( -7.700916879387133607E-14, 12.51293083811828843, -20.85287692521917080 ) ) ;
#8883 = CARTESIAN_POINT ( 'NONE',  ( 93.63799900313688340, -2.337932895214617890, -2.000000000000000888 ) ) ;
#8884 = LINE ( 'NONE', #14892, #8569 ) ;
#8885 = PLANE ( 'NONE',  #5892 ) ;
#8886 = CYLINDRICAL_SURFACE ( 'NONE', #1823, 13.19999999999999929 ) ;
#8887 = EDGE_CURVE ( 'NONE', #10221, #3461, #7328, .T. ) ;
#8888 = EDGE_CURVE ( 'NONE', #5940, #14085, #11451, .T. ) ;
#8889 = ORIENTED_EDGE ( 'NONE', *, *, #331, .T. ) ;
#8891 = CIRCLE ( 'NONE', #11350, 2.524999999999996358 ) ;
#8890 = CARTESIAN_POINT ( 'NONE',  ( 1.749999999999999778, 4.458161950358745074, -17.39253030560836777 ) ) ;
#8892 = CIRCLE ( 'NONE', #3009, 2.524999999999996358 ) ;
#8893 = EDGE_CURVE ( 'NONE', #13265, #4412, #8692, .T. ) ;
#8894 = CARTESIAN_POINT ( 'NONE',  ( -5.999999999999999112, 0.000000000000000000, 5.500000000000000000 ) ) ;
#8895 = CARTESIAN_POINT ( 'NONE',  ( 2.789999999999999147, -24.15498966839958683, -5.391175441198872598 ) ) ;
#8896 = VERTEX_POINT ( 'NONE', #9782 ) ;
#8897 = DIRECTION ( 'NONE',  ( 1.000000000000000000, 0.000000000000000000, -0.000000000000000000 ) ) ;
#8898 = DIRECTION ( 'NONE',  ( 0.000000000000000000, 0.000000000000000000, 1.000000000000000000 ) ) ;
#8899 = ORIENTED_EDGE ( 'NONE', *, *, #13238, .F. ) ;
#8900 = ORIENTED_EDGE ( 'NONE', *, *, #14987, .T. ) ;
#8901 = CARTESIAN_POINT ( 'NONE',  ( -10.00000000000000000, 0.000000000000000000, 0.000000000000000000 ) ) ;
#8902 = DIRECTION ( 'NONE',  ( 0.000000000000000000, -1.717547996016640980E-15, -1.000000000000000000 ) ) ;
#8903 = CIRCLE ( 'NONE', #14806, 9.999999999999994671 ) ;
#8904 = MANIFOLD_SOLID_BREP ( 'Bore', #7575 ) ;
#8905 = CARTESIAN_POINT ( 'NONE',  ( 2.789999999999999147, 0.000000000000000000, 0.000000000000000000 ) ) ;
#8906 = LINE ( 'NONE', #14535, #9420 ) ;
#8907 = FACE_OUTER_BOUND ( 'NONE', #11914, .T. ) ;
#8908 = EDGE_CURVE ( 'NONE', #11392, #7854, #3323, .T. ) ;
#8909 = CARTESIAN_POINT ( 'NONE',  ( 0.02436607992776411782, 22.71065055754465689, -9.836394144775473691 ) ) ;
#8910 = LINE ( 'NONE', #12452, #11589 ) ;
#8911 = EDGE_CURVE ( 'NONE', #15059, #12037, #7628, .T. ) ;
#8912 = ORIENTED_EDGE ( 'NONE', *, *, #1126, .T. ) ;
#8913 = B_SPLINE_CURVE_WITH_KNOTS ( 'NONE', 3,
 ( #2650, #7344, #1492, #6176, #12314, #2094 ),
 .UNSPECIFIED., .F., .F.,
 ( 4, 2, 4 ),
 ( 4.462636732872785396E-07, 0.001879885066975069564, 0.003759323870276851630 ),
 .UNSPECIFIED. ) ;
#8914 = DIRECTION ( 'NONE',  ( -0.9140840597599245720, -0.4055247608874392728, 9.273332052389774862E-17 ) ) ;
#8915 = B_SPLINE_CURVE_WITH_KNOTS ( 'NONE', 3,
 ( #10203, #6603, #11423, #3284 ),
 .UNSPECIFIED., .F., .F.,
 ( 4, 4 ),
 ( 3.059063720746924101E-07, 0.0006888942284913933487 ),
 .UNSPECIFIED. ) ;
#8916 = CARTESIAN_POINT ( 'NONE',  ( 1.039999999999997593, 4.835383649608715473, -17.29145405592683815 ) ) ;
#8917 = VERTEX_POINT ( 'NONE', #14550 ) ;
#8918 = EDGE_CURVE ( 'NONE', #12675, #5309, #9695, .T. ) ;
#8919 =( LENGTH_UNIT ( ) NAMED_UNIT ( * ) SI_UNIT ( .MILLI., .METRE. ) );
#8920 = ORIENTED_EDGE ( 'NONE', *, *, #13134, .F. ) ;
#8921 = VERTEX_POINT ( 'NONE', #6397 ) ;
#8922 = ORIENTED_EDGE ( 'NONE', *, *, #3452, .T. ) ;
#8923 = LINE ( 'NONE', #4009, #6029 ) ;
#8924 = DIRECTION ( 'NONE',  ( 0.000000000000000000, 0.000000000000000000, 1.000000000000000000 ) ) ;
#8925 = CARTESIAN_POINT ( 'NONE',  ( 0.02531912748606228100, 5.229914364928351489, 13.68080036884350292 ) ) ;
#8926 = CARTESIAN_POINT ( 'NONE',  ( 56.98919079003883326, 3.953582723775848962, 7.000000000000000000 ) ) ;
#8927 = VERTEX_POINT ( 'NONE', #9920 ) ;
#8928 = DIRECTION ( 'NONE',  ( 0.000000000000000000, 0.000000000000000000, -1.000000000000000000 ) ) ;
#8929 = CYLINDRICAL_SURFACE ( 'NONE', #11720, 5.575000000000000178 ) ;
#8930 = VERTEX_POINT ( 'NONE', #2274 ) ;
#8931 = CARTESIAN_POINT ( 'NONE',  ( 1.039999999999997593, -12.52377138324241557, 25.12109765559648977 ) ) ;
#8932 = CARTESIAN_POINT ( 'NONE',  ( 1.039999999999997593, 0.000000000000000000, 0.000000000000000000 ) ) ;
#8933 = AXIS2_PLACEMENT_3D ( 'NONE', #784, #4184, #5493 ) ;
#8934 = AXIS2_PLACEMENT_3D ( 'NONE', #7175, #3484, #14019 ) ;
#8935 = ORIENTED_EDGE ( 'NONE', *, *, #10029, .T. ) ;
#8936 = DIRECTION ( 'NONE',  ( 1.000000000000000000, 0.000000000000000000, 0.000000000000000000 ) ) ;
#8937 = CARTESIAN_POINT ( 'NONE',  ( 0.02531912748286561932, 13.68080036884348516, 5.229914364928400339 ) ) ;
#8938 = AXIS2_PLACEMENT_3D ( 'NONE', #6875, #7742, #4216 ) ;
#8939 = ORIENTED_EDGE ( 'NONE', *, *, #4388, .F. ) ;
#8940 = ORIENTED_EDGE ( 'NONE', *, *, #453, .T. ) ;
#8941 = DIRECTION ( 'NONE',  ( -0.000000000000000000, -0.000000000000000000, -1.000000000000000000 ) ) ;
#8942 = LINE ( 'NONE', #13719, #11417 ) ;
#8943 = AXIS2_PLACEMENT_3D ( 'NONE', #11294, #5468, #1698 ) ;
#8944 = ORIENTED_EDGE ( 'NONE', *, *, #8068, .T. ) ;
#8945 = MECHANICAL_DESIGN_GEOMETRIC_PRESENTATION_REPRESENTATION (  '', ( #7722 ), #6249 ) ;
#8946 = CARTESIAN_POINT ( 'NONE',  ( 2.790000000000000924, 0.000000000000000000, 0.000000000000000000 ) ) ;
#8947 = B_SPLINE_CURVE_WITH_KNOTS ( 'NONE', 3,
 ( #11126, #13592, #9766, #6453 ),
 .UNSPECIFIED., .F., .F.,
 ( 4, 4 ),
 ( 1.981826382900849143E-07, 0.0006887856082032012620 ),
 .UNSPECIFIED. ) ;
#8948 = ADVANCED_FACE ( 'NONE', ( #14778 ), #3943, .F. ) ;
#8949 = VERTEX_POINT ( 'NONE', #4010 ) ;
#8950 = DIRECTION ( 'NONE',  ( 1.000000000000000000, 0.000000000000000000, 0.000000000000000000 ) ) ;
#8951 = ORIENTED_EDGE ( 'NONE', *, *, #10388, .T. ) ;
#8952 = CARTESIAN_POINT ( 'NONE',  ( 2.789999999999999147, 13.40591150984226587, 7.739906618939754956 ) ) ;
#8953 = DIRECTION ( 'NONE',  ( -0.6310987668242443727, -0.7757024858236036824, -5.947623346206206400E-19 ) ) ;
#8954 = ORIENTED_EDGE ( 'NONE', *, *, #4440, .F. ) ;
#8955 = AXIS2_PLACEMENT_3D ( 'NONE', #15043, #3277, #5670 ) ;
#8956 = CIRCLE ( 'NONE', #14862, 28.06981291497571007 ) ;
#8957 = ORIENTED_EDGE ( 'NONE', *, *, #12834, .T. ) ;
#8958 = DIRECTION ( 'NONE',  ( -1.000000000000000000, -0.000000000000000000, -0.000000000000000000 ) ) ;
#8959 = EDGE_CURVE ( 'NONE', #1894, #12582, #3014, .T. ) ;
#8960 = CARTESIAN_POINT ( 'NONE',  ( 98.33955663538051795, 3.898681236723621879, -2.000000000000000888 ) ) ;
#8961 = DIRECTION ( 'NONE',  ( -1.000000000000000000, -0.000000000000000000, -0.000000000000000000 ) ) ;
#8962 = SHAPE_DEFINITION_REPRESENTATION ( #10326, #1017 ) ;
#8963 = DIRECTION ( 'NONE',  ( 1.000000000000000000, 0.000000000000000000, 0.000000000000000000 ) ) ;
#8964 = EDGE_CURVE ( 'NONE', #9957, #9499, #8956, .T. ) ;
#8965 = CARTESIAN_POINT ( 'NONE',  ( 2.781248467066446572, 13.40591150985955871, -5.214906618939568972 ) ) ;
#8966 = DIRECTION ( 'NONE',  ( 0.000000000000000000, 0.000000000000000000, 1.000000000000000000 ) ) ;
#8967 = CIRCLE ( 'NONE', #9703, 2.999999999999975131 ) ;
#8968 = ORIENTED_EDGE ( 'NONE', *, *, #2802, .F. ) ;
#8969 = PLANE ( 'NONE',  #8306 ) ;
#8970 = CIRCLE ( 'NONE', #5318, 4.000000000000000000 ) ;
#8971 = B_SPLINE_CURVE_WITH_KNOTS ( 'NONE', 3,
 ( #4281, #5448, #11494, #13961 ),
 .UNSPECIFIED., .F., .F.,
 ( 4, 4 ),
 ( 1.984117560508715598E-07, 0.0009182716802120147702 ),
 .UNSPECIFIED. ) ;
#8972 = LINE ( 'NONE', #7829, #2498 ) ;
#8973 = EDGE_CURVE ( 'NONE', #4472, #4704, #8619, .T. ) ;
#8974 = CARTESIAN_POINT ( 'NONE',  ( 2.765633920072235963, -16.37294372382871188, 18.55949924794887096 ) ) ;
#8975 = EDGE_LOOP ( 'NONE', ( #3608, #10967, #4297, #6756, #6861, #10652 ) ) ;
#8976 = CARTESIAN_POINT ( 'NONE',  ( 2.789999999999999147, 5.535312321042718864, 23.48180575137732262 ) ) ;
#8977 = CARTESIAN_POINT ( 'NONE',  ( 0.02436607992776411782, -16.37294372382844543, -18.55949924794910544 ) ) ;
#8978 = ORIENTED_EDGE ( 'NONE', *, *, #12161, .T. ) ;
#8979 = ORIENTED_EDGE ( 'NONE', *, *, #14455, .F. ) ;
#8980 = CARTESIAN_POINT ( 'NONE',  ( 2.765633920072242624, -22.71065055754459650, 9.836394144775621129 ) ) ;
#8981 = AXIS2_PLACEMENT_3D ( 'NONE', #595, #5233, #11058 ) ;
#8982 = DIRECTION ( 'NONE',  ( 0.000000000000000000, 0.000000000000000000, -1.000000000000000000 ) ) ;
#8983 = EDGE_CURVE ( 'NONE', #11249, #5438, #14012, .T. ) ;
#8984 = DIRECTION ( 'NONE',  ( 0.000000000000000000, 0.000000000000000000, -1.000000000000000000 ) ) ;
#8985 = DIRECTION ( 'NONE',  ( 0.000000000000000000, 0.000000000000000000, 1.000000000000000000 ) ) ;
#8986 = DIRECTION ( 'NONE',  ( 0.000000000000000000, 0.9510565162951498674, 0.3090169943749583870 ) ) ;
#8987 = FACE_OUTER_BOUND ( 'NONE', #10441, .T. ) ;
#8988 = CARTESIAN_POINT ( 'NONE',  ( 2.789999999999999147, -9.999777909379854890, -11.07980565117290794 ) ) ;
#8989 = EDGE_LOOP ( 'NONE', ( #4467, #235, #7765, #12102, #5654, #3892 ) ) ;
#8990 = CIRCLE ( 'NONE', #11442, 4.000000000000000000 ) ;
#8991 = CARTESIAN_POINT ( 'NONE',  ( 1.039999999999999147, -17.39253030560838198, -4.458161950358684678 ) ) ;
#8992 = EDGE_CURVE ( 'NONE', #6712, #2078, #2831, .T. ) ;
#8993 = VECTOR ( 'NONE', #3714, 1000.000000000000000 ) ;
#8994 = DIRECTION ( 'NONE',  ( -0.000000000000000000, -0.000000000000000000, -1.000000000000000000 ) ) ;
#8995 = ORIENTED_EDGE ( 'NONE', *, *, #9107, .F. ) ;
#8996 = PRESENTATION_LAYER_ASSIGNMENT (  '', '', ( #9242 ) ) ;
#8997 = EDGE_CURVE ( 'NONE', #241, #13926, #7862, .T. ) ;
#8998 = EDGE_LOOP ( 'NONE', ( #14275, #2896, #14520, #15101 ) ) ;
#8999 = ORIENTED_EDGE ( 'NONE', *, *, #14005, .F. ) ;
#9000 = ORIENTED_EDGE ( 'NONE', *, *, #1194, .T. ) ;
#9001 = CARTESIAN_POINT ( 'NONE',  ( 0.02531912748606271468, -5.229914364928256454, -13.68080036884353845 ) ) ;
#9002 = EDGE_CURVE ( 'NONE', #9526, #7097, #11901, .T. ) ;
#9003 = SURFACE_STYLE_FILL_AREA ( #15009 ) ;
#9004 = EDGE_CURVE ( 'NONE', #6879, #12150, #8798, .T. ) ;
#9005 = AXIS2_PLACEMENT_3D ( 'NONE', #4748, #6046, #14115 ) ;
#9006 = VECTOR ( 'NONE', #6230, 1000.000000000000114 ) ;
#9007 = MECHANICAL_DESIGN_GEOMETRIC_PRESENTATION_REPRESENTATION (  '', ( #7781 ), #9997 ) ;
#9008 = DIRECTION ( 'NONE',  ( -1.000000000000000000, -0.000000000000000000, -0.000000000000000000 ) ) ;
#9009 = CIRCLE ( 'NONE', #3127, 4.872650870659752442 ) ;
#9010 = ORIENTED_EDGE ( 'NONE', *, *, #2577, .T. ) ;
#9011 = DIRECTION ( 'NONE',  ( 0.000000000000000000, 0.000000000000000000, 1.000000000000000000 ) ) ;
#9012 = CARTESIAN_POINT ( 'NONE',  ( 2.789999999999999147, -23.48180575137726223, -5.535312321042966666 ) ) ;
#9013 = CARTESIAN_POINT ( 'NONE',  ( 0.6549552265645784965, 16.44225436089927683, 5.086950209440548321 ) ) ;
#9014 = CIRCLE ( 'NONE', #10735, 11.66666666666667318 ) ;
#9015 = ADVANCED_FACE ( 'NONE', ( #11378 ), #5485, .F. ) ;
#9016 = LINE ( 'NONE', #6784, #5479 ) ;
#9017 = EDGE_CURVE ( 'NONE', #12081, #389, #11267, .T. ) ;
#9018 = AXIS2_PLACEMENT_3D ( 'NONE', #1062, #6976, #5756 ) ;
#9019 = VERTEX_POINT ( 'NONE', #13998 ) ;
#9020 = VECTOR ( 'NONE', #3495, 1000.000000000000000 ) ;
#9021 = CARTESIAN_POINT ( 'NONE',  ( 0.000000000000000000, 13.87420763704361626, 1.948757464274225137 ) ) ;
#9022 = LINE ( 'NONE', #721, #11651 ) ;
#9023 = ADVANCED_FACE ( 'NONE', ( #12826 ), #9760, .T. ) ;
#9024 = CIRCLE ( 'NONE', #8776, 28.06981291497571007 ) ;
#9025 = ORIENTED_EDGE ( 'NONE', *, *, #14570, .F. ) ;
#9026 = EDGE_LOOP ( 'NONE', ( #4736, #308, #4974, #5991, #12502, #14574 ) ) ;
#9027 = AXIS2_PLACEMENT_3D ( 'NONE', #8946, #12327, #13637 ) ;
#9028 = DIRECTION ( 'NONE',  ( 0.000000000000000000, 0.000000000000000000, -1.000000000000000000 ) ) ;
#9029 = EDGE_CURVE ( 'NONE', #13750, #12819, #7058, .T. ) ;
#9030 = ORIENTED_EDGE ( 'NONE', *, *, #3701, .F. ) ;
#9031 = VECTOR ( 'NONE', #6856, 1000.000000000000000 ) ;
#9032 = CARTESIAN_POINT ( 'NONE',  ( 2.789999999999999147, -0.2301004812055740811, -24.44424927289185590 ) ) ;
#9033 = ORIENTED_EDGE ( 'NONE', *, *, #4019, .F. ) ;
#9034 = CARTESIAN_POINT ( 'NONE',  ( 2.789999999999999147, -5.391175441198450713, -24.15498966839968276 ) ) ;
#9035 = CARTESIAN_POINT ( 'NONE',  ( 0.008751532933531189218, -13.40591150985895297, -5.214906618939850524 ) ) ;
#9036 = AXIS2_PLACEMENT_3D ( 'NONE', #12806, #10592, #5840 ) ;
#9037 = CIRCLE ( 'NONE', #6583, 2.524999999999998579 ) ;
#9038 = ORIENTED_EDGE ( 'NONE', *, *, #11003, .F. ) ;
#9039 = SURFACE_STYLE_USAGE ( .BOTH. , #12712 ) ;
#9040 = MANIFOLD_SOLID_BREP ( 'Bore', #1082 ) ;
#9041 = DIRECTION ( 'NONE',  ( 0.000000000000000000, 5.496153587253259026E-15, -1.000000000000000000 ) ) ;
#9042 = ORIENTED_EDGE ( 'NONE', *, *, #3186, .T. ) ;
#9043 = ORIENTED_EDGE ( 'NONE', *, *, #4399, .T. ) ;
#9044 = CIRCLE ( 'NONE', #1184, 2.524999999999999467 ) ;
#9045 = DIRECTION ( 'NONE',  ( -1.445602896647338917E-16, 1.000000000000000000, -0.000000000000000000 ) ) ;
#9046 = CARTESIAN_POINT ( 'NONE',  ( 1.398397006336996817, -6.091550361990593743, -0.8000000000000000444 ) ) ;
#9047 = CARTESIAN_POINT ( 'NONE',  ( 18.71314632718394222, -23.25585687728512241, 2.000000000000000000 ) ) ;
#9048 = VECTOR ( 'NONE', #179, 1000.000000000000114 ) ;
#9049 = CARTESIAN_POINT ( 'NONE',  ( 10.40394475573011945, -10.79473832354794460, 5.500000000000000000 ) ) ;
#9050 = ITEM_DEFINED_TRANSFORMATION ( 'NONE', 'NONE', #4521,  #1376 ) ;
#9051 = AXIS2_PLACEMENT_3D ( 'NONE', #1806, #6580, #12560 ) ;
#9052 = DIRECTION ( 'NONE',  ( 0.8893705212896308998, -0.4571871344001384729, 0.000000000000000000 ) ) ;
#9053 = CARTESIAN_POINT ( 'NONE',  ( 0.5279273620711150139, 23.73240184472514613, -12.96450951081191150 ) ) ;
#9054 = B_SPLINE_CURVE_WITH_KNOTS ( 'NONE', 3,
 ( #8937, #1797, #6482, #13628 ),
 .UNSPECIFIED., .F., .F.,
 ( 4, 4 ),
 ( 1.988537750524637048E-07, 0.0006916721208754034915 ),
 .UNSPECIFIED. ) ;
#9055 = ORIENTED_EDGE ( 'NONE', *, *, #9748, .T. ) ;
#9056 = CARTESIAN_POINT ( 'NONE',  ( 2.765633920072239516, -24.63872515616084513, 2.336989772644183283 ) ) ;
#9057 = CARTESIAN_POINT ( 'NONE',  ( 75.20570977803312473, 12.97982004111159959, 7.000000000000000000 ) ) ;
#9058 = CARTESIAN_POINT ( 'NONE',  ( 2.789999999999999147, -24.34211360614294506, -7.909232158575071558 ) ) ;
#9059 = ORIENTED_EDGE ( 'NONE', *, *, #10617, .F. ) ;
#9060 = AXIS2_PLACEMENT_3D ( 'NONE', #4681, #4909, #2213 ) ;
#9061 = CIRCLE ( 'NONE', #9027, 4.000000000000000000 ) ;
#9062 = CIRCLE ( 'NONE', #2433, 2.524999999999996803 ) ;
#9063 = EDGE_CURVE ( 'NONE', #10155, #14360, #12682, .T. ) ;
#9064 = CARTESIAN_POINT ( 'NONE',  ( 2.790000000000077751, 5.456611084821854085, 23.69897269326679279 ) ) ;
#9065 = CARTESIAN_POINT ( 'NONE',  ( 2.789999999999999147, -24.44424927289185590, 0.2301004812056573479 ) ) ;
#9066 = EDGE_LOOP ( 'NONE', ( #10938, #2259, #3011, #12993 ) ) ;
#9067 = VERTEX_POINT ( 'NONE', #3245 ) ;
#9068 = CARTESIAN_POINT ( 'NONE',  ( 0.04999671820202215150, 5.264737421541719975, -13.99876742897254012 ) ) ;
#9069 = CARTESIAN_POINT ( 'NONE',  ( 2.789999999999999147, -5.249430348645663713, -12.98979500319699731 ) ) ;
#9070 = VERTEX_POINT ( 'NONE', #15161 ) ;
#9071 = DIRECTION ( 'NONE',  ( -0.000000000000000000, -0.000000000000000000, -1.000000000000000000 ) ) ;
#9072 = CARTESIAN_POINT ( 'NONE',  ( 1.749999999999999778, -4.835383649608351320, -17.29145405592693763 ) ) ;
#9073 = DIRECTION ( 'NONE',  ( -1.000000000000000000, -0.000000000000000000, -0.000000000000000000 ) ) ;
#9074 = CARTESIAN_POINT ( 'NONE',  ( 0.7592463834391194322, -24.80264696524891477, 12.05220173035428921 ) ) ;
#9075 = CARTESIAN_POINT ( 'NONE',  ( 0.7589665349472715095, 27.14933624560914893, -4.828387785247743480 ) ) ;
#9076 = AXIS2_PLACEMENT_3D ( 'NONE', #1847, #13680, #11297 ) ;
#9077 = ORIENTED_EDGE ( 'NONE', *, *, #12184, .T. ) ;
#9078 = DIRECTION ( 'NONE',  ( -1.000000000000000000, -0.000000000000000000, -0.000000000000000000 ) ) ;
#9079 = CARTESIAN_POINT ( 'NONE',  ( 1.249999999999997558, 0.000000000000000000, 0.000000000000000000 ) ) ;
#9080 = ORIENTED_EDGE ( 'NONE', *, *, #9480, .F. ) ;
#9081 = ORIENTED_EDGE ( 'NONE', *, *, #8629, .F. ) ;
#9082 = ORIENTED_EDGE ( 'NONE', *, *, #3910, .T. ) ;
#9083 = EDGE_LOOP ( 'NONE', ( #13071, #12688, #5955, #8818 ) ) ;
#9084 = AXIS2_PLACEMENT_3D ( 'NONE', #1450, #14589, #5157 ) ;
#9085 = CARTESIAN_POINT ( 'NONE',  ( 2.764680872513937349, -13.68080036884344963, -5.229914364928496262 ) ) ;
#9086 =( NAMED_UNIT ( * ) PLANE_ANGLE_UNIT ( ) SI_UNIT ( $, .RADIAN. ) );
#9087 = ADVANCED_FACE ( 'NONE', ( #1081 ), #2876, .T. ) ;
#9088 = DIRECTION ( 'NONE',  ( -5.339417856040273846E-17, -1.063174570779084847E-17, 1.000000000000000000 ) ) ;
#9089 = CARTESIAN_POINT ( 'NONE',  ( 2.718131853594929037, -12.74240566898999383, 21.92302674874958868 ) ) ;
#9090 = ORIENTED_EDGE ( 'NONE', *, *, #140, .F. ) ;
#9091 = PLANE ( 'NONE',  #12436 ) ;
#9092 = CARTESIAN_POINT ( 'NONE',  ( 66.02295749185037721, 31.67615731643408949, 2.000000000000000000 ) ) ;
#9093 = B_SPLINE_CURVE_WITH_KNOTS ( 'NONE', 3,
 ( #5634, #12604, #10379, #9001 ),
 .UNSPECIFIED., .F., .F.,
 ( 4, 4 ),
 ( 0.005123742438166226966, 0.005814376014856854902 ),
 .UNSPECIFIED. ) ;
#9094 = VECTOR ( 'NONE', #15124, 1000.000000000000000 ) ;
#9095 = PRODUCT_RELATED_PRODUCT_CATEGORY ( 'part', '', ( #10699 ) ) ;
#9096 = EDGE_CURVE ( 'NONE', #11359, #14141, #11463, .T. ) ;
#9097 = ADVANCED_FACE ( 'NONE', ( #1009 ), #14710, .T. ) ;
#9098 = CARTESIAN_POINT ( 'NONE',  ( 1.039999999999996483, 4.147968289691283950, 27.76164181293052735 ) ) ;
#9099 = ORIENTED_EDGE ( 'NONE', *, *, #12674, .T. ) ;
#9100 = CARTESIAN_POINT ( 'NONE',  ( 0.1855657389739094887, -5.253342437939553022, -25.39738473785006079 ) ) ;
#9101 = FACE_OUTER_BOUND ( 'NONE', #14150, .T. ) ;
#9102 = ORIENTED_EDGE ( 'NONE', *, *, #14959, .T. ) ;
#9103 = ORIENTED_EDGE ( 'NONE', *, *, #1044, .F. ) ;
#9104 =( NAMED_UNIT ( * ) PLANE_ANGLE_UNIT ( ) SI_UNIT ( $, .RADIAN. ) );
#9105 = CARTESIAN_POINT ( 'NONE',  ( 2.789999999999999147, -7.909232158574647009, -24.34211360614308006 ) ) ;
#9106 = EDGE_CURVE ( 'NONE', #2082, #9825, #14209, .T. ) ;
#9107 = EDGE_CURVE ( 'NONE', #10848, #860, #7969, .T. ) ;
#9108 = ORIENTED_EDGE ( 'NONE', *, *, #12489, .T. ) ;
#9109 = CARTESIAN_POINT ( 'NONE',  ( 15.21482963846748504, 16.90833299098317610, -130.1575142076926852 ) ) ;
#9110 =( REPRESENTATION_RELATIONSHIP ('NONE','NONE', #12685, #7313 ) REPRESENTATION_RELATIONSHIP_WITH_TRANSFORMATION ( #5521 )SHAPE_REPRESENTATION_RELATIONSHIP( ) );
#9111 = EDGE_CURVE ( 'NONE', #4155, #13280, #217, .T. ) ;
#9112 = CARTESIAN_POINT ( 'NONE',  ( 2.718184767880471142, 10.24584646439571500, -23.19431517146922417 ) ) ;
#9113 = DIRECTION ( 'NONE',  ( -1.000000000000000000, -0.000000000000000000, -0.000000000000000000 ) ) ;
#9114 = ORIENTED_EDGE ( 'NONE', *, *, #7877, .F. ) ;
#9115 = LINE ( 'NONE', #13568, #6314 ) ;
#9116 = DIRECTION ( 'NONE',  ( 0.5416238976136762417, -0.8406209333187997235, 0.000000000000000000 ) ) ;
#9117 = VERTEX_POINT ( 'NONE', #3611 ) ;
#9118 = B_SPLINE_CURVE_WITH_KNOTS ( 'NONE', 3,
 ( #12365, #9074, #10299, #3162, #6762, #11217 ),
 .UNSPECIFIED., .F., .F.,
 ( 4, 2, 4 ),
 ( 4.462636882236601199E-07, 0.001879885203074806947, 0.003759324142461389993 ),
 .UNSPECIFIED. ) ;
#9119 = EDGE_CURVE ( 'NONE', #4384, #2817, #3760, .T. ) ;
#9120 = EDGE_LOOP ( 'NONE', ( #5855, #537, #12303, #11355 ) ) ;
#9121 = DIRECTION ( 'NONE',  ( -0.9148936170212769170, -0.4036950204470262649, 0.000000000000000000 ) ) ;
#9122 = FACE_OUTER_BOUND ( 'NONE', #13584, .T. ) ;
#9123 = CARTESIAN_POINT ( 'NONE',  ( 1.749999999999998002, 4.633866840649310426, -27.68468304288254345 ) ) ;
#9124 = CARTESIAN_POINT ( 'NONE',  ( 0.7592463977762147209, -4.828194074574546413, 27.14986936243572657 ) ) ;
#9125 = CONTEXT_DEPENDENT_SHAPE_REPRESENTATION ( #1542, #13016 ) ;
#9126 = FACE_OUTER_BOUND ( 'NONE', #10259, .T. ) ;
#9127 = FACE_OUTER_BOUND ( 'NONE', #10061, .T. ) ;
#9128 = ORIENTED_EDGE ( 'NONE', *, *, #11130, .T. ) ;
#9129 = CYLINDRICAL_SURFACE ( 'NONE', #14711, 2.524999999999998579 ) ;
#9130 = CARTESIAN_POINT ( 'NONE',  ( 2.789999999999999147, 15.04425356660760293, 20.70663861606276868 ) ) ;
#9131 = DIRECTION ( 'NONE',  ( 0.000000000000000000, 0.000000000000000000, 1.000000000000000000 ) ) ;
#9132 = AXIS2_PLACEMENT_3D ( 'NONE', #10649, #101, #4824 ) ;
#9133 = EDGE_LOOP ( 'NONE', ( #8700, #10794 ) ) ;
#9134 = DIRECTION ( 'NONE',  ( 0.000000000000000000, 0.000000000000000000, 1.000000000000000000 ) ) ;
#9135 = CARTESIAN_POINT ( 'NONE',  ( 72.49759028996471955, 17.18292470770558822, -2.000000000000000888 ) ) ;
#9136 = ORIENTED_EDGE ( 'NONE', *, *, #8106, .T. ) ;
#9137 = ORIENTED_EDGE ( 'NONE', *, *, #8825, .T. ) ;
#9138 = CARTESIAN_POINT ( 'NONE',  ( 0.02531912748464674665, 5.229914364928542447, -13.68080036884343009 ) ) ;
#9139 = CARTESIAN_POINT ( 'NONE',  ( 2.718131864678290821, 25.22589920183360945, -2.577209017047097372 ) ) ;
#9140 = ORIENTED_EDGE ( 'NONE', *, *, #6102, .T. ) ;
#9141 = CARTESIAN_POINT ( 'NONE',  ( 2.790000000000078639, 15.96555658743789152, -18.34439787333489136 ) ) ;
#9142 = LINE ( 'NONE', #15061, #14100 ) ;
#9143 = DIRECTION ( 'NONE',  ( 0.000000000000000000, 0.000000000000000000, 1.000000000000000000 ) ) ;
#9144 = CIRCLE ( 'NONE', #6935, 11.66666666666667318 ) ;
#9145 = CARTESIAN_POINT ( 'NONE',  ( 0.5321745087963410947, 24.44564404695860205, -11.58891744060082019 ) ) ;
#9146 = CARTESIAN_POINT ( 'NONE',  ( 0.04387302227425586565, -0.8988970056815597243, 4.000000000000000000 ) ) ;
#9147 = ORIENTED_EDGE ( 'NONE', *, *, #5784, .T. ) ;
#9148 = LINE ( 'NONE', #921, #2120 ) ;
#9149 = DIRECTION ( 'NONE',  ( 0.000000000000000000, -1.224646799147353207E-16, 1.000000000000000000 ) ) ;
#9150 = ADVANCED_FACE ( 'NONE', ( #5930 ), #4618, .T. ) ;
#9151 = ORIENTED_EDGE ( 'NONE', *, *, #8992, .T. ) ;
#9152 = VECTOR ( 'NONE', #1518, 1000.000000000000000 ) ;
#9153 = ORIENTED_EDGE ( 'NONE', *, *, #14930, .F. ) ;
#9154 = EDGE_LOOP ( 'NONE', ( #4471, #5505, #4706, #6629 ) ) ;
#9155 = EDGE_LOOP ( 'NONE', ( #14224, #9651, #1458, #13482 ) ) ;
#9156 = CARTESIAN_POINT ( 'NONE',  ( 98.48580539929344013, 0.9022481406819604643, 4.000000000000000000 ) ) ;
#9157 = DIRECTION ( 'NONE',  ( -1.000000000000000000, -0.000000000000000000, -0.000000000000000000 ) ) ;
#9158 = DIRECTION ( 'NONE',  ( 0.1643989873053573469, -0.9863939238321437486, 0.000000000000000000 ) ) ;
#9159 = EDGE_CURVE ( 'NONE', #860, #5525, #1741, .T. ) ;
#9160 = CARTESIAN_POINT ( 'NONE',  ( -10.97587178374205941, -9.155129925568431304, -3.000000000000000444 ) ) ;
#9161 = EDGE_CURVE ( 'NONE', #214, #3838, #14672, .T. ) ;
#9162 = ORIENTED_EDGE ( 'NONE', *, *, #972, .F. ) ;
#9163 = CARTESIAN_POINT ( 'NONE',  ( 2.783068888626318405, 9.685942809247050533, 22.53293026234507579 ) ) ;
#9164 = DIRECTION ( 'NONE',  ( -0.4571871344001416926, -0.8893705212896291235, -0.000000000000000000 ) ) ;
#9165 = EDGE_CURVE ( 'NONE', #1485, #3479, #13927, .T. ) ;
#9166 = CARTESIAN_POINT ( 'NONE',  ( 1.039999999999997149, 17.39253030560841751, -4.458161950358562997 ) ) ;
#9167 = ORIENTED_EDGE ( 'NONE', *, *, #4004, .F. ) ;
#9168 = DIRECTION ( 'NONE',  ( 1.000000000000000000, 0.000000000000000000, 0.000000000000000000 ) ) ;
#9169 = CARTESIAN_POINT ( 'NONE',  ( 2.789999999999999147, 15.04425356660790136, -18.18163861606255338 ) ) ;
#9170 = ORIENTED_EDGE ( 'NONE', *, *, #9649, .T. ) ;
#9171 = ORIENTED_EDGE ( 'NONE', *, *, #12489, .F. ) ;
#9172 = EDGE_CURVE ( 'NONE', #15013, #7167, #11825, .T. ) ;
#9173 = EDGE_CURVE ( 'NONE', #4864, #3507, #5995, .T. ) ;
#9174 = CARTESIAN_POINT ( 'NONE',  ( -10.00000000000000000, 0.000000000000000000, 0.000000000000000000 ) ) ;
#9175 =( GEOMETRIC_REPRESENTATION_CONTEXT ( 3 ) GLOBAL_UNCERTAINTY_ASSIGNED_CONTEXT ( ( #4094 ) ) GLOBAL_UNIT_ASSIGNED_CONTEXT ( ( #10539, #9312, #14138 ) ) REPRESENTATION_CONTEXT ( 'NONE', 'WORKASPACE' ) );
#9176 = VERTEX_POINT ( 'NONE', #2387 ) ;
#9177 = CARTESIAN_POINT ( 'NONE',  ( 2.031033479673592268, -19.86422722021325882, 19.12621924769859660 ) ) ;
#9178 = CARTESIAN_POINT ( 'NONE',  ( 0.1882238552569852619, 10.68696068830407420, 23.64332819722385182 ) ) ;
#9179 = VECTOR ( 'NONE', #7253, 1000.000000000000114 ) ;
#9180 = AXIS2_PLACEMENT_3D ( 'NONE', #240, #7769, #10711 ) ;
#9181 = ORIENTED_EDGE ( 'NONE', *, *, #14063, .F. ) ;
#9182 = DIRECTION ( 'NONE',  ( -0.000000000000000000, -0.000000000000000000, 1.000000000000000000 ) ) ;
#9183 = AXIS2_PLACEMENT_3D ( 'NONE', #11621, #10123, #14818 ) ;
#9184 = CARTESIAN_POINT ( 'NONE',  ( 0.09203966225861176520, 2.583706482362034151, 15.03709480088672734 ) ) ;
#9185 = ORIENTED_EDGE ( 'NONE', *, *, #12019, .T. ) ;
#9186 = ADVANCED_FACE ( 'NONE', ( #10684, #136 ), #8528, .F. ) ;
#9187 = EDGE_CURVE ( 'NONE', #12416, #9424, #10978, .T. ) ;
#9188 = VERTEX_POINT ( 'NONE', #2616 ) ;
#9189 = CARTESIAN_POINT ( 'NONE',  ( -14.40394475573011945, -10.79473832354794283, -3.799999999999999822 ) ) ;
#9191 = FACE_OUTER_BOUND ( 'NONE', #9155, .T. ) ;
#9190 = VECTOR ( 'NONE', #4534, 1000.000000000000000 ) ;
#9192 = EDGE_CURVE ( 'NONE', #1378, #3632, #10033, .T. ) ;
#9193 = EDGE_CURVE ( 'NONE', #7336, #14793, #6076, .T. ) ;
#9194 = VECTOR ( 'NONE', #837, 1000.000000000000000 ) ;
#9195 = LINE ( 'NONE', #10273, #12467 ) ;
#9196 = CIRCLE ( 'NONE', #2559, 31.62277660168379256 ) ;
#9197 = APPLICATION_CONTEXT ( 'automotive_design' ) ;
#9198 = DIRECTION ( 'NONE',  ( 0.000000000000000000, 0.000000000000000000, 1.000000000000000000 ) ) ;
#9199 = LINE ( 'NONE', #6962, #2933 ) ;
#9200 = DIRECTION ( 'NONE',  ( 5.782411586589355667E-16, 1.000000000000000000, -0.000000000000000000 ) ) ;
#9201 = VERTEX_POINT ( 'NONE', #10764 ) ;
#9202 = FACE_OUTER_BOUND ( 'NONE', #3028, .T. ) ;
#9203 = CARTESIAN_POINT ( 'NONE',  ( 64.00448238961524794, 36.25062540154047497, -2.000000000000000000 ) ) ;
#9204 = VECTOR ( 'NONE', #12423, 1000.000000000000000 ) ;
#9205 = CARTESIAN_POINT ( 'NONE',  ( 2.789999999999999147, 20.70663861606293210, -15.04425356660737556 ) ) ;
#9206 = AXIS2_PLACEMENT_3D ( 'NONE', #12997, #7098, #9470 ) ;
#9207 = ORIENTED_EDGE ( 'NONE', *, *, #15037, .T. ) ;
#9208 = CIRCLE ( 'NONE', #346, 2.524999999999997247 ) ;
#9209 = CARTESIAN_POINT ( 'NONE',  ( -19.40394475573011590, -4.794738323547945491, 16.99999999999999645 ) ) ;
#9210 = LINE ( 'NONE', #9135, #9467 ) ;
#9211 = VERTEX_POINT ( 'NONE', #14298 ) ;
#9212 = ORIENTED_EDGE ( 'NONE', *, *, #2721, .T. ) ;
#9213 = CARTESIAN_POINT ( 'NONE',  ( 0.2076373605413179835, 5.278564329441211456, -14.94126095370955731 ) ) ;
#9214 = DIRECTION ( 'NONE',  ( -1.000000000000000000, -0.000000000000000000, -0.000000000000000000 ) ) ;
#9215 = EDGE_LOOP ( 'NONE', ( #8441, #7712, #9910, #5587, #818 ) ) ;
#9216 = DIRECTION ( 'NONE',  ( 1.000000000000000000, 0.000000000000000000, 0.000000000000000000 ) ) ;
#9217 = DIRECTION ( 'NONE',  ( 1.000000000000000000, 0.000000000000000000, 0.000000000000000000 ) ) ;
#9218 = DIRECTION ( 'NONE',  ( 0.000000000000000000, 0.000000000000000000, 1.000000000000000000 ) ) ;
#9219 = AXIS2_PLACEMENT_3D ( 'NONE', #10331, #2030, #6715 ) ;
#9220 = CIRCLE ( 'NONE', #2344, 14.01039946648073986 ) ;
#9221 = AXIS2_PLACEMENT_3D ( 'NONE', #7010, #2183, #13782 ) ;
#9222 = DIRECTION ( 'NONE',  ( 0.000000000000000000, 0.000000000000000000, 1.000000000000000000 ) ) ;
#9223 = CARTESIAN_POINT ( 'NONE',  ( 2.724374482943360487, 21.84204283372364230, 12.72258903105646688 ) ) ;
#9224 = EDGE_CURVE ( 'NONE', #11407, #13089, #53, .T. ) ;
#9225 = ORIENTED_EDGE ( 'NONE', *, *, #13904, .T. ) ;
#9226 = CARTESIAN_POINT ( 'NONE',  ( 2.789999999999999147, 23.48180575137730131, 5.535312321042802353 ) ) ;
#9227 = ORIENTED_EDGE ( 'NONE', *, *, #6087, .F. ) ;
#9228 = VERTEX_POINT ( 'NONE', #3996 ) ;
#9229 = ORIENTED_EDGE ( 'NONE', *, *, #7210, .T. ) ;
#9230 = ORIENTED_EDGE ( 'NONE', *, *, #13267, .T. ) ;
#9231 = DIRECTION ( 'NONE',  ( 0.000000000000000000, 0.000000000000000000, -1.000000000000000000 ) ) ;
#9232 = SURFACE_STYLE_USAGE ( .BOTH. , #14853 ) ;
#9233 = EDGE_CURVE ( 'NONE', #12264, #12279, #10770, .T. ) ;
#9234 = PLANE ( 'NONE',  #2170 ) ;
#9235 = DIRECTION ( 'NONE',  ( 0.000000000000000000, 0.000000000000000000, 1.000000000000000000 ) ) ;
#9236 = EDGE_CURVE ( 'NONE', #11663, #2567, #4301, .T. ) ;
#9237 = UNCERTAINTY_MEASURE_WITH_UNIT (LENGTH_MEASURE( 1.000000000000000082E-05 ), #12640, 'distance_accuracy_value', 'NONE');
#9238 = DIRECTION ( 'NONE',  ( 0.000000000000000000, -1.000000000000000000, 0.000000000000000000 ) ) ;
#9239 = AXIS2_PLACEMENT_3D ( 'NONE', #3149, #1994, #14827 ) ;
#9240 = ORIENTED_EDGE ( 'NONE', *, *, #7895, .F. ) ;
#9241 = CARTESIAN_POINT ( 'NONE',  ( 2.765633920072242624, 9.836394144775706394, 22.71065055754456097 ) ) ;
#9242 = STYLED_ITEM ( 'NONE', ( #13535 ), #8180 ) ;
#9243 = B_SPLINE_CURVE_WITH_KNOTS ( 'NONE', 3,
 ( #6292, #11201, #1756, #676 ),
 .UNSPECIFIED., .F., .F.,
 ( 4, 4 ),
 ( 1.988537749986050620E-07, 0.0002742066915197750193 ),
 .UNSPECIFIED. ) ;
#9244 = CARTESIAN_POINT ( 'NONE',  ( 0.02531912748256377743, 14.46287784598617421, -2.311161484776606212 ) ) ;
#9245 = EDGE_CURVE ( 'NONE', #14739, #8589, #7613, .T. ) ;
#9246 = CIRCLE ( 'NONE', #14887, 3.799999999999999378 ) ;
#9247 = ORIENTED_EDGE ( 'NONE', *, *, #47, .T. ) ;
#9248 = DIRECTION ( 'NONE',  ( 0.000000000000000000, 0.000000000000000000, 1.000000000000000000 ) ) ;
#9249 = AXIS2_PLACEMENT_3D ( 'NONE', #9940, #2792, #11165 ) ;
#9250 = EDGE_CURVE ( 'NONE', #1278, #2195, #3927, .T. ) ;
#9251 = CARTESIAN_POINT ( 'NONE',  ( 2.764680872513208598, 11.36963888406700285, -9.232963481057645083 ) ) ;
#9252 = ORIENTED_EDGE ( 'NONE', *, *, #6365, .T. ) ;
#9253 = ORIENTED_EDGE ( 'NONE', *, *, #6864, .F. ) ;
#9254 = VECTOR ( 'NONE', #12358, 1000.000000000000000 ) ;
#9255 = CARTESIAN_POINT ( 'NONE',  ( 1.039999999999997593, 0.000000000000000000, 0.000000000000000000 ) ) ;
#9256 = ORIENTED_EDGE ( 'NONE', *, *, #13839, .F. ) ;
#9257 = VECTOR ( 'NONE', #4046, 1000.000000000000000 ) ;
#9258 = CARTESIAN_POINT ( 'NONE',  ( 2.764680872515352661, 9.232963481057920418, -11.36963888406677725 ) ) ;
#9259 = CARTESIAN_POINT ( 'NONE',  ( 2.789999999999999147, -11.04103753892277417, 8.624777288397760699 ) ) ;
#9260 = CARTESIAN_POINT ( 'NONE',  ( 0.001865824574860882289, 20.90825775245787455, -12.51925356660738053 ) ) ;
#9261 = DIRECTION ( 'NONE',  ( 0.000000000000000000, 0.000000000000000000, 1.000000000000000000 ) ) ;
#9262 = VECTOR ( 'NONE', #14812, 1000.000000000000000 ) ;
#9263 = ORIENTED_EDGE ( 'NONE', *, *, #8360, .F. ) ;
#9264 = AXIS2_PLACEMENT_3D ( 'NONE', #12643, #887, #3276 ) ;
#9265 = CARTESIAN_POINT ( 'NONE',  ( 0.000000000000000000, 0.000000000000000000, 3.895000000000000462 ) ) ;
#9266 = FACE_OUTER_BOUND ( 'NONE', #5255, .T. ) ;
#9267 = AXIS2_PLACEMENT_3D ( 'NONE', #11213, #11292, #2144 ) ;
#9268 = ORIENTED_EDGE ( 'NONE', *, *, #3248, .F. ) ;
#9269 = ORIENTED_EDGE ( 'NONE', *, *, #7138, .F. ) ;
#9270 = CARTESIAN_POINT ( 'NONE',  ( 0.000000000000000000, 5.249430348645932831, -12.98979500319689251 ) ) ;
#9271 = DIRECTION ( 'NONE',  ( 0.000000000000000000, 1.374038396813314756E-15, -1.000000000000000000 ) ) ;
#9272 = ADVANCED_FACE ( 'NONE', ( #13361 ), #4111, .T. ) ;
#9273 = AXIS2_PLACEMENT_3D ( 'NONE', #14121, #4831, #3587 ) ;
#9274 = DIRECTION ( 'NONE',  ( 0.000000000000000000, 0.000000000000000000, 1.000000000000000000 ) ) ;
#9275 = CARTESIAN_POINT ( 'NONE',  ( 2.789999999999999147, 24.15498966839963302, 5.391175441198700291 ) ) ;
#9276 = ITEM_DEFINED_TRANSFORMATION ( 'NONE', 'NONE', #8214,  #1376 ) ;
#9277 = CIRCLE ( 'NONE', #13932, 28.06981291497571362 ) ;
#9278 = CARTESIAN_POINT ( 'NONE',  ( 0.007327532539343941352, 14.24942254254686169, -2.217238903388591087 ) ) ;
#9279 = AXIS2_PLACEMENT_3D ( 'NONE', #810, #11341, #15041 ) ;
#9280 = AXIS2_PLACEMENT_3D ( 'NONE', #14717, #11315, #1718 ) ;
#9281 = LINE ( 'NONE', #10424, #9094 ) ;
#9282 = VERTEX_POINT ( 'NONE', #8831 ) ;
#9283 = CARTESIAN_POINT ( 'NONE',  ( 80.00000000000000000, 0.000000000000000000, 5.500000000000000000 ) ) ;
#9284 = CARTESIAN_POINT ( 'NONE',  ( 80.00000000000000000, 0.000000000000000000, 5.500000000000000000 ) ) ;
#9285 = DIRECTION ( 'NONE',  ( -1.000000000000000000, -0.000000000000000000, -0.000000000000000000 ) ) ;
#9286 = CARTESIAN_POINT ( 'NONE',  ( 0.02436607992775978102, 16.37294372382885044, -18.55949924794875017 ) ) ;
#9287 = EDGE_CURVE ( 'NONE', #8287, #8724, #8035, .T. ) ;
#9288 = EDGE_CURVE ( 'NONE', #11326, #2590, #6567, .T. ) ;
#9289 = ORIENTED_EDGE ( 'NONE', *, *, #8292, .T. ) ;
#9290 = LINE ( 'NONE', #246, #8993 ) ;
#9291 = CARTESIAN_POINT ( 'NONE',  ( 0.04925989934398850717, -13.98927362834336918, 5.263697681271511719 ) ) ;
#9292 = ORIENTED_EDGE ( 'NONE', *, *, #2254, .T. ) ;
#9293 = AXIS2_PLACEMENT_3D ( 'NONE', #1980, #3212, #10048 ) ;
#9294 = ORIENTED_EDGE ( 'NONE', *, *, #5062, .T. ) ;
#9295 = AXIS2_PLACEMENT_3D ( 'NONE', #5964, #3502, #10426 ) ;
#9296 = CARTESIAN_POINT ( 'NONE',  ( 0.09203962824862059466, 9.756102650610241511, 11.73065272960066707 ) ) ;
#9297 = CARTESIAN_POINT ( 'NONE',  ( 60.64109936584995353, 31.48746944824151583, -2.000000000000000000 ) ) ;
#9298 = ORIENTED_EDGE ( 'NONE', *, *, #9550, .F. ) ;
#9299 = CARTESIAN_POINT ( 'NONE',  ( 2.789999999999999147, 15.74360496233408213, -18.28042085475260592 ) ) ;
#9300 = DIRECTION ( 'NONE',  ( 0.000000000000000000, 0.000000000000000000, 1.000000000000000000 ) ) ;
#9301 = CARTESIAN_POINT ( 'NONE',  ( 0.000000000000000000, 0.000000000000000000, 5.500000000000000000 ) ) ;
#9302 = DIRECTION ( 'NONE',  ( 0.000000000000000000, 0.000000000000000000, -1.000000000000000000 ) ) ;
#9303 = DIRECTION ( 'NONE',  ( -0.000000000000000000, 1.000000000000000000, 0.000000000000000000 ) ) ;
#9304 = EDGE_CURVE ( 'NONE', #7716, #14810, #4152, .T. ) ;
#9305 = ADVANCED_FACE ( 'NONE', ( #13525 ), #13591, .F. ) ;
#9306 = ORIENTED_EDGE ( 'NONE', *, *, #7393, .F. ) ;
#9307 = CARTESIAN_POINT ( 'NONE',  ( 0.000000000000000000, -12.52067188844335988, -20.62201879784928238 ) ) ;
#9308 = AXIS2_PLACEMENT_3D ( 'NONE', #9580, #7275, #5057 ) ;
#9309 = CARTESIAN_POINT ( 'NONE',  ( 2.789999999999999147, 0.000000000000000000, 0.000000000000000000 ) ) ;
#9310 = EDGE_CURVE ( 'NONE', #14933, #15005, #4158, .T. ) ;
#9311 = ORIENTED_EDGE ( 'NONE', *, *, #4419, .T. ) ;
#9312 =( NAMED_UNIT ( * ) PLANE_ANGLE_UNIT ( ) SI_UNIT ( $, .RADIAN. ) );
#9313 = ORIENTED_EDGE ( 'NONE', *, *, #752, .F. ) ;
#9314 = ORIENTED_EDGE ( 'NONE', *, *, #5178, .T. ) ;
#9315 = ORIENTED_EDGE ( 'NONE', *, *, #12813, .T. ) ;
#9316 = CARTESIAN_POINT ( 'NONE',  ( 1.749999999999998002, -12.52377138324241734, 25.12109765559649688 ) ) ;
#9317 = DIRECTION ( 'NONE',  ( -1.000000000000000000, -0.000000000000000000, -0.000000000000000000 ) ) ;
#9318 = EDGE_CURVE ( 'NONE', #13854, #552, #11988, .T. ) ;
#9319 = CARTESIAN_POINT ( 'NONE',  ( 1.749999999999999778, -4.835383649608351320, -17.29145405592693763 ) ) ;
#9320 = DIRECTION ( 'NONE',  ( 1.000000000000000000, 0.000000000000000000, 0.000000000000000000 ) ) ;
#9321 = CARTESIAN_POINT ( 'NONE',  ( 0.5279273746168620107, 4.996265754456365116, 26.57710921259763026 ) ) ;
#9322 = EDGE_LOOP ( 'NONE', ( #843, #7012 ) ) ;
#9323 = CARTESIAN_POINT ( 'NONE',  ( 1.039999999999996483, -27.76164181293054511, 4.147968289691193355 ) ) ;
#9324 = AXIS2_PLACEMENT_3D ( 'NONE', #3, #5785, #1388 ) ;
#9325 = ORIENTED_EDGE ( 'NONE', *, *, #11542, .T. ) ;
#9326 = DIRECTION ( 'NONE',  ( 0.000000000000000000, 0.000000000000000000, -1.000000000000000000 ) ) ;
#9327 = CARTESIAN_POINT ( 'NONE',  ( 1.387778780781445676E-14, 0.000000000000000000, -7.000000000000007994 ) ) ;
#9328 = ORIENTED_EDGE ( 'NONE', *, *, #5091, .F. ) ;
#9329 = EDGE_LOOP ( 'NONE', ( #3868, #3002, #12735, #2533 ) ) ;
#9330 = EDGE_CURVE ( 'NONE', #8861, #1742, #1404, .T. ) ;
#9331 = CARTESIAN_POINT ( 'NONE',  ( -14.40394475573011945, -10.79473832354794460, -3.794707603699265519E-15 ) ) ;
#9332 = AXIS2_PLACEMENT_3D ( 'NONE', #1127, #7042, #12792 ) ;
#9333 = ORIENTED_EDGE ( 'NONE', *, *, #13267, .F. ) ;
#9334 = CARTESIAN_POINT ( 'NONE',  ( 2.508169608347904145, 15.25429862889489208, -5.259531939870039530 ) ) ;
#9335 = CARTESIAN_POINT ( 'NONE',  ( -7.728448779411724935E-14, -2.133839912090635949, -24.22524813288764989 ) ) ;
#9336 = EDGE_CURVE ( 'NONE', #3644, #1400, #10906, .T. ) ;
#9337 = LINE ( 'NONE', #11557, #2803 ) ;
#9338 = ORIENTED_EDGE ( 'NONE', *, *, #12382, .T. ) ;
#9339 = CARTESIAN_POINT ( 'NONE',  ( -1.250000000000001110, 0.000000000000000000, -5.899999999999999467 ) ) ;
#9340 = DIRECTION ( 'NONE',  ( 0.000000000000000000, 0.000000000000000000, 1.000000000000000000 ) ) ;
#9341 = ORIENTED_EDGE ( 'NONE', *, *, #3195, .T. ) ;
#9342 = ORIENTED_EDGE ( 'NONE', *, *, #12554, .F. ) ;
#9343 = CARTESIAN_POINT ( 'NONE',  ( 67.45386469005195806, 13.93318132202354676, 2.999999999999999112 ) ) ;
#9344 = CARTESIAN_POINT ( 'NONE',  ( 2.789999999999999147, -15.47981323787947794, -1.080949580976661932E-13 ) ) ;
#9345 = CARTESIAN_POINT ( 'NONE',  ( 2.783025228907523019, 9.686319561461266048, -22.53337530003393141 ) ) ;
#9346 = FACE_OUTER_BOUND ( 'NONE', #12854, .T. ) ;
#9347 = CARTESIAN_POINT ( 'NONE',  ( -14.40394475573011945, -7.794738323547949044, 22.00000000000000000 ) ) ;
#9348 = CARTESIAN_POINT ( 'NONE',  ( 2.765633920072239516, -24.63872515616084513, 2.336989772644183283 ) ) ;
#9349 = EDGE_CURVE ( 'NONE', #6574, #8927, #5842, .T. ) ;
#9350 = EDGE_LOOP ( 'NONE', ( #6254, #9328, #14449, #6702, #11867, #13284 ) ) ;
#9351 = CYLINDRICAL_SURFACE ( 'NONE', #698, 13.20000000000000284 ) ;
#9352 = DIRECTION ( 'NONE',  ( -1.000000000000000000, 0.000000000000000000, 0.000000000000000000 ) ) ;
#9353 = CARTESIAN_POINT ( 'NONE',  ( 0.000000000000000000, 11.04103753892283635, -8.624777288397693198 ) ) ;
#9354 = CARTESIAN_POINT ( 'NONE',  ( 2.765633920072235963, 22.71065055754452544, 9.836394144775786330 ) ) ;
#9355 = ORIENTED_EDGE ( 'NONE', *, *, #15037, .F. ) ;
#9356 = EDGE_CURVE ( 'NONE', #797, #7388, #8764, .T. ) ;
#9357 = VERTEX_POINT ( 'NONE', #11125 ) ;
#9358 = EDGE_LOOP ( 'NONE', ( #12894, #8178, #9252, #9042, #6395, #7831 ) ) ;
#9359 = FACE_OUTER_BOUND ( 'NONE', #8361, .T. ) ;
#9360 = DIRECTION ( 'NONE',  ( 0.000000000000000000, 0.000000000000000000, 1.000000000000000000 ) ) ;
#9361 = DIRECTION ( 'NONE',  ( 0.000000000000000000, 0.000000000000000000, 1.000000000000000000 ) ) ;
#9362 = CARTESIAN_POINT ( 'NONE',  ( 0.000000000000000000, 11.04103753892283635, -8.624777288397693198 ) ) ;
#9363 = CARTESIAN_POINT ( 'NONE',  ( -4.872650870659752442, 0.4273491293402474911, 0.000000000000000000 ) ) ;
#9364 = EDGE_CURVE ( 'NONE', #677, #14436, #6224, .T. ) ;
#9365 = ADVANCED_FACE ( 'NONE', ( #599 ), #5317, .T. ) ;
#9366 = CARTESIAN_POINT ( 'NONE',  ( 0.07186813532171117125, -25.22589920183359169, -2.577209017047271011 ) ) ;
#9367 = FACE_OUTER_BOUND ( 'NONE', #3372, .T. ) ;
#9368 = ORIENTED_EDGE ( 'NONE', *, *, #9615, .T. ) ;
#9369 = CARTESIAN_POINT ( 'NONE',  ( 93.34550147531103903, 3.654933296868752457, 7.000000000000000000 ) ) ;
#9370 = CARTESIAN_POINT ( 'NONE',  ( -1.249999999999997780, 5.021051876504148371E-16, 4.100000000000000533 ) ) ;
#9371 = ORIENTED_EDGE ( 'NONE', *, *, #10049, .F. ) ;
#9372 = VERTEX_POINT ( 'NONE', #8063 ) ;
#9373 = VERTEX_POINT ( 'NONE', #6832 ) ;
#9374 = ORIENTED_EDGE ( 'NONE', *, *, #11437, .F. ) ;
#9375 = DIRECTION ( 'NONE',  ( -1.000000000000000000, -0.000000000000000000, -0.000000000000000000 ) ) ;
#9376 = EDGE_CURVE ( 'NONE', #10254, #14234, #12542, .T. ) ;
#9377 = CARTESIAN_POINT ( 'NONE',  ( 0.5537796329733301048, -5.139875429511743476, -16.15122426806993872 ) ) ;
#9378 = DIRECTION ( 'NONE',  ( 0.000000000000000000, 0.000000000000000000, 1.000000000000000000 ) ) ;
#9379 = CYLINDRICAL_SURFACE ( 'NONE', #10522, 3.799999999999999378 ) ;
#9380 = EDGE_CURVE ( 'NONE', #4433, #8382, #5538, .T. ) ;
#9381 = CARTESIAN_POINT ( 'NONE',  ( 2.246812931352481169, 12.54666350726123447, 11.42270873787296992 ) ) ;
#9382 = ORIENTED_EDGE ( 'NONE', *, *, #13311, .F. ) ;
#9383 = DIRECTION ( 'NONE',  ( 1.000000000000000000, 0.000000000000000000, 0.000000000000000000 ) ) ;
#9384 = EDGE_CURVE ( 'NONE', #1181, #5498, #7303, .T. ) ;
#9385 = CIRCLE ( 'NONE', #2522, 3.000000000000002665 ) ;
#9386 =( REPRESENTATION_RELATIONSHIP ('NONE','NONE', #12685, #7313 ) REPRESENTATION_RELATIONSHIP_WITH_TRANSFORMATION ( #3653 )SHAPE_REPRESENTATION_RELATIONSHIP( ) );
#9387 = VERTEX_POINT ( 'NONE', #7757 ) ;
#9388 = CARTESIAN_POINT ( 'NONE',  ( -19.40394475573011590, -4.794738323547945491, 22.00000000000000000 ) ) ;
#9389 = CARTESIAN_POINT ( 'NONE',  ( 0.07181525696555274285, -24.78695292654917637, -5.344212458769628249 ) ) ;
#9390 = ORIENTED_EDGE ( 'NONE', *, *, #3929, .T. ) ;
#9391 = VERTEX_POINT ( 'NONE', #12738 ) ;
#9392 = CIRCLE ( 'NONE', #5490, 2.524999999999999467 ) ;
#9393 = DIRECTION ( 'NONE',  ( 0.7573544145849104847, -0.6530040510661075936, -2.081668171172168513E-17 ) ) ;
#9394 = ORIENTED_EDGE ( 'NONE', *, *, #14137, .F. ) ;
#9395 = DIRECTION ( 'NONE',  ( -1.000000000000000000, 0.000000000000000000, 0.000000000000000000 ) ) ;
#9396 = DIRECTION ( 'NONE',  ( -1.000000000000000000, -0.000000000000000000, -0.000000000000000000 ) ) ;
#9397 = DIRECTION ( 'NONE',  ( 0.000000000000000000, 0.000000000000000000, 1.000000000000000000 ) ) ;
#9398 = DIRECTION ( 'NONE',  ( 1.000000000000000000, 0.000000000000000000, 0.000000000000000000 ) ) ;
#9399 = EDGE_LOOP ( 'NONE', ( #8056, #1716, #5192, #4952, #4653, #3864 ) ) ;
#9400 = DIRECTION ( 'NONE',  ( 1.000000000000000000, 0.000000000000000000, -0.000000000000000000 ) ) ;
#9401 = CARTESIAN_POINT ( 'NONE',  ( 0.1920563539683071974, 2.883512197589228165, -15.58455734132163251 ) ) ;
#9402 = VERTEX_POINT ( 'NONE', #9297 ) ;
#9403 = ORIENTED_EDGE ( 'NONE', *, *, #386, .T. ) ;
#9404 = DIRECTION ( 'NONE',  ( 1.000000000000000000, 0.000000000000000000, 0.000000000000000000 ) ) ;
#9405 = DIRECTION ( 'NONE',  ( 0.000000000000000000, 0.000000000000000000, 1.000000000000000000 ) ) ;
#9406 = AXIS2_PLACEMENT_3D ( 'NONE', #13197, #13033, #12964 ) ;
#9407 = CARTESIAN_POINT ( 'NONE',  ( 1.387778780781445676E-14, 0.000000000000000000, -7.800000000000008704 ) ) ;
#9408 = CARTESIAN_POINT ( 'NONE',  ( 0.006931038682727013421, -21.08061549536624568, 12.53626894672821201 ) ) ;
#9409 = DIRECTION ( 'NONE',  ( -1.000000000000000000, 0.000000000000000000, 0.000000000000000000 ) ) ;
#9410 = EDGE_CURVE ( 'NONE', #7166, #13214, #12906, .T. ) ;
#9411 = CARTESIAN_POINT ( 'NONE',  ( -9.999999999999998224, -1.390791565672605534, 6.000000000000000000 ) ) ;
#9412 = ORIENTED_EDGE ( 'NONE', *, *, #8615, .F. ) ;
#9413 = CARTESIAN_POINT ( 'NONE',  ( 1.039999999999995817, -27.76164181293048472, -4.147968289691575272 ) ) ;
#9414 = AXIS2_PLACEMENT_3D ( 'NONE', #12113, #2909, #11116 ) ;
#9415 = CYLINDRICAL_SURFACE ( 'NONE', #785, 6.000000000000005329 ) ;
#9416 = CARTESIAN_POINT ( 'NONE',  ( 0.5321745227542249435, 18.57583492944418779, 19.66801664102709779 ) ) ;
#9417 = CARTESIAN_POINT ( 'NONE',  ( 0.000000000000000000, 0.4273491293402468805, -0.8000000000000000444 ) ) ;
#9418 = ORIENTED_EDGE ( 'NONE', *, *, #4306, .F. ) ;
#9419 = ORIENTED_EDGE ( 'NONE', *, *, #8911, .F. ) ;
#9420 = VECTOR ( 'NONE', #7542, 1000.000000000000000 ) ;
#9421 = EDGE_CURVE ( 'NONE', #5016, #8792, #13979, .T. ) ;
#9422 = CARTESIAN_POINT ( 'NONE',  ( 0.7589665283900991488, 27.31260702007175567, 3.797536611356412628 ) ) ;
#9423 = VECTOR ( 'NONE', #6174, 1000.000000000000000 ) ;
#9424 = VERTEX_POINT ( 'NONE', #10139 ) ;
#9425 = CIRCLE ( 'NONE', #2805, 0.5999999999999998668 ) ;
#9426 = CARTESIAN_POINT ( 'NONE',  ( 1.749999999999999778, 12.83329210556849453, -12.55714665599973578 ) ) ;
#9427 = DIRECTION ( 'NONE',  ( -1.000000000000000000, 0.000000000000000000, 0.000000000000000000 ) ) ;
#9428 = ADVANCED_FACE ( 'NONE', ( #764 ), #12446, .T. ) ;
#9429 = LINE ( 'NONE', #1445, #2142 ) ;
#9430 = CARTESIAN_POINT ( 'NONE',  ( 0.007327564474061625845, 11.23174270417341880, -9.044896821682087307 ) ) ;
#9431 = DIRECTION ( 'NONE',  ( -0.000000000000000000, -0.000000000000000000, 1.000000000000000000 ) ) ;
#9432 = ADVANCED_FACE ( 'NONE', ( #15058 ), #4300, .T. ) ;
#9433 = LINE ( 'NONE', #14129, #2458 ) ;
#9434 = VECTOR ( 'NONE', #2391, 1000.000000000000000 ) ;
#9435 = VECTOR ( 'NONE', #14245, 1000.000000000000000 ) ;
#9436 = ORIENTED_EDGE ( 'NONE', *, *, #4867, .F. ) ;
#9437 = CARTESIAN_POINT ( 'NONE',  ( 1.039999999999996705, -20.02152543075331081, -19.67366047555552555 ) ) ;
#9438 = DIRECTION ( 'NONE',  ( -1.000000000000000000, -0.000000000000000000, -0.000000000000000000 ) ) ;
#9439 = AXIS2_PLACEMENT_3D ( 'NONE', #5094, #9769, #454 ) ;
#9440 = DIRECTION ( 'NONE',  ( 1.445602896647338917E-16, -1.000000000000000000, 0.000000000000000000 ) ) ;
#9441 = EDGE_LOOP ( 'NONE', ( #10557, #8725, #11525, #10656 ) ) ;
#9442 = EDGE_CURVE ( 'NONE', #1149, #3935, #11473, .T. ) ;
#9443 = SHAPE_REPRESENTATION_RELATIONSHIP ( 'NONE' , 'NONE' ,  #7891, #675 ) ;
#9444 = AXIS2_PLACEMENT_3D ( 'NONE', #14443, #8356, #8587 ) ;
#9445 = ORIENTED_EDGE ( 'NONE', *, *, #15079, .T. ) ;
#9446 = ORIENTED_EDGE ( 'NONE', *, *, #1285, .F. ) ;
#9447 = VERTEX_POINT ( 'NONE', #13673 ) ;
#9448 = CARTESIAN_POINT ( 'NONE',  ( 2.764680872513208598, 11.36963888406700285, -9.232963481057645083 ) ) ;
#9449 = VECTOR ( 'NONE', #4836, 1000.000000000000000 ) ;
#9450 = CARTESIAN_POINT ( 'NONE',  ( 80.00000000000000000, 0.000000000000000000, 5.500000000000005329 ) ) ;
#9451 = CYLINDRICAL_SURFACE ( 'NONE', #4374, 2.524999999999999467 ) ;
#9452 = CARTESIAN_POINT ( 'NONE',  ( 1.749999999999999778, -4.458161950358622505, 17.39253030560840330 ) ) ;
#9453 = ADVANCED_FACE ( 'NONE', ( #12523 ), #4616, .T. ) ;
#9454 = CARTESIAN_POINT ( 'NONE',  ( 1.039999999999995817, 4.633866840648921404, 27.68468304288260029 ) ) ;
#9455 = ORIENTED_EDGE ( 'NONE', *, *, #7976, .T. ) ;
#9456 = FACE_OUTER_BOUND ( 'NONE', #13977, .T. ) ;
#9457 = AXIS2_PLACEMENT_3D ( 'NONE', #4427, #6872, #2410 ) ;
#9458 = EDGE_CURVE ( 'NONE', #8188, #6679, #388, .T. ) ;
#9459 = EDGE_CURVE ( 'NONE', #2812, #10393, #2065, .T. ) ;
#9460 = ADVANCED_FACE ( 'NONE', ( #11362 ), #3228, .T. ) ;
#9461 = ORIENTED_EDGE ( 'NONE', *, *, #4325, .F. ) ;
#9462 = CARTESIAN_POINT ( 'NONE',  ( 0.000000000000000000, 0.000000000000000000, 0.000000000000000000 ) ) ;
#9463 = PRODUCT ( 'hub', 'hub', '', ( #2906 ) ) ;
#9464 = DIRECTION ( 'NONE',  ( 0.1305261922200521840, 0.9914448613738103822, 0.000000000000000000 ) ) ;
#9465 = ORIENTED_EDGE ( 'NONE', *, *, #8049, .F. ) ;
#9466 = ORIENTED_EDGE ( 'NONE', *, *, #14379, .F. ) ;
#9467 = VECTOR ( 'NONE', #12440, 1000.000000000000000 ) ;
#9468 = LINE ( 'NONE', #6016, #10683 ) ;
#9469 = ORIENTED_EDGE ( 'NONE', *, *, #10826, .T. ) ;
#9470 = DIRECTION ( 'NONE',  ( 0.000000000000000000, 0.000000000000000000, 1.000000000000000000 ) ) ;
#9471 = CARTESIAN_POINT ( 'NONE',  ( 1.394999999999998685, 20.02152543075374425, -19.67366047555508857 ) ) ;
#9472 = EDGE_CURVE ( 'NONE', #11571, #9661, #9024, .T. ) ;
#9473 = EDGE_CURVE ( 'NONE', #10254, #11686, #909, .T. ) ;
#9474 = DIRECTION ( 'NONE',  ( -1.000000000000000000, 0.000000000000000000, -0.000000000000000000 ) ) ;
#9475 = CIRCLE ( 'NONE', #11923, 28.06981291497571007 ) ;
#9476 = DIRECTION ( 'NONE',  ( -0.000000000000000000, -0.000000000000000000, -1.000000000000000000 ) ) ;
#9477 = ORIENTED_EDGE ( 'NONE', *, *, #8444, .T. ) ;
#9478 = VECTOR ( 'NONE', #1332, 1000.000000000000000 ) ;
#9479 = CARTESIAN_POINT ( 'NONE',  ( 1.749999999999998002, 0.000000000000000000, 0.000000000000000000 ) ) ;
#9480 = EDGE_CURVE ( 'NONE', #5284, #6485, #5371, .T. ) ;
#9481 = B_SPLINE_CURVE_WITH_KNOTS ( 'NONE', 3,
 ( #10267, #11265, #4274, #803, #3205, #15034 ),
 .UNSPECIFIED., .F., .F.,
 ( 4, 2, 4 ),
 ( 4.462636695652347161E-07, 0.001879885036799764601, 0.003759323809929963987 ),
 .UNSPECIFIED. ) ;
#9482 = B_SPLINE_CURVE_WITH_KNOTS ( 'NONE', 3,
 ( #11020, #9864, #9799, #14640 ),
 .UNSPECIFIED., .F., .F.,
 ( 4, 4 ),
 ( 0.005258139959819246867, 0.005948405594583413246 ),
 .UNSPECIFIED. ) ;
#9483 = CARTESIAN_POINT ( 'NONE',  ( 1.394999999999999574, 12.96210679857786552, 24.89775460606837143 ) ) ;
#9484 = COLOUR_RGB ( '',1.000000000000000000, 0.9490196078431372140, 0.9098039215686274384 ) ;
#9485 = AXIS2_PLACEMENT_3D ( 'NONE', #2197, #2340, #8250 ) ;
#9486 = ORIENTED_EDGE ( 'NONE', *, *, #8052, .F. ) ;
#9487 = EDGE_LOOP ( 'NONE', ( #2105, #8851, #14943, #3286 ) ) ;
#9488 = CARTESIAN_POINT ( 'NONE',  ( -1.249999999999997780, 0.000000000000000000, -4.100000000000000533 ) ) ;
#9489 = DIRECTION ( 'NONE',  ( -5.480158469902919838E-17, -1.051478716308701618E-16, -1.000000000000000000 ) ) ;
#9490 = ADVANCED_FACE ( 'NONE', ( #2517 ), #7283, .T. ) ;
#9491 = CIRCLE ( 'NONE', #14663, 0.1000000000000011297 ) ;
#9492 = CARTESIAN_POINT ( 'NONE',  ( 2.765633920072235519, 9.836394144776026138, -22.71065055754441531 ) ) ;
#9493 = CARTESIAN_POINT ( 'NONE',  ( 72.68384697807672978, 11.35494834827056110, 7.000000000000000000 ) ) ;
#9494 = ITEM_DEFINED_TRANSFORMATION ( 'NONE', 'NONE', #10188,  #1376 ) ;
#9495 = CARTESIAN_POINT ( 'NONE',  ( 0.007349531976027940186, -2.217353748342030695, 14.24968354755767663 ) ) ;
#9496 = CIRCLE ( 'NONE', #654, 5.400000000000000355 ) ;
#9497 = CARTESIAN_POINT ( 'NONE',  ( 0.000000000000000000, 0.000000000000000000, 6.000000000000000000 ) ) ;
#9498 = VECTOR ( 'NONE', #1219, 1000.000000000000000 ) ;
#9499 = VERTEX_POINT ( 'NONE', #14333 ) ;
#9500 = CARTESIAN_POINT ( 'NONE',  ( 0.000000000000000000, -11.04103753892277417, 8.624777288397769581 ) ) ;
#9501 = CARTESIAN_POINT ( 'NONE',  ( 76.00000000000000000, 4.898587196589420717E-16, -130.1575142076926852 ) ) ;
#9502 = AXIS2_PLACEMENT_3D ( 'NONE', #14604, #14533, #5090 ) ;
#9503 = FACE_OUTER_BOUND ( 'NONE', #11850, .T. ) ;
#9504 = CARTESIAN_POINT ( 'NONE',  ( 0.000000000000000000, 8.624777288397959651, -11.04103753892262674 ) ) ;
#9505 = MECHANICAL_DESIGN_GEOMETRIC_PRESENTATION_REPRESENTATION (  '', ( #7551 ), #1163 ) ;
#9506 = ORIENTED_EDGE ( 'NONE', *, *, #13431, .T. ) ;
#9507 = ORIENTED_EDGE ( 'NONE', *, *, #6468, .F. ) ;
#9508 = ORIENTED_EDGE ( 'NONE', *, *, #12061, .T. ) ;
#9509 = PRESENTATION_LAYER_ASSIGNMENT (  '', '', ( #7558 ) ) ;
#9510 = DIRECTION ( 'NONE',  ( -1.000000000000000000, -0.000000000000000000, -0.000000000000000000 ) ) ;
#9511 = LINE ( 'NONE', #12960, #414 ) ;
#9512 = AXIS2_PLACEMENT_3D ( 'NONE', #6039, #2886, #14423 ) ;
#9513 = CARTESIAN_POINT ( 'NONE',  ( 1.039999999999996927, 4.835383649608473000, 17.29145405592690565 ) ) ;
#9514 = DIRECTION ( 'NONE',  ( 0.000000000000000000, 0.8090169943749527803, -0.5877852522924655876 ) ) ;
#9515 = DIRECTION ( 'NONE',  ( 0.000000000000000000, 0.000000000000000000, -1.000000000000000000 ) ) ;
#9516 = CARTESIAN_POINT ( 'NONE',  ( 2.141980652367355464, -6.189445006155633422, 0.000000000000000000 ) ) ;
#9517 = ORIENTED_EDGE ( 'NONE', *, *, #1784, .T. ) ;
#9518 = CARTESIAN_POINT ( 'NONE',  ( 1.039999999999997371, -4.147968289691092991, -27.76164181293055933 ) ) ;
#9519 = LINE ( 'NONE', #3596, #12372 ) ;
#9520 = ORIENTED_EDGE ( 'NONE', *, *, #12220, .T. ) ;
#9521 = CARTESIAN_POINT ( 'NONE',  ( 1.666666666666673624, 0.000000000000000000, -131.1575142076926852 ) ) ;
#9522 = DIRECTION ( 'NONE',  ( 0.000000000000000000, 0.000000000000000000, 1.000000000000000000 ) ) ;
#9523 = AXIS2_PLACEMENT_3D ( 'NONE', #13079, #13252, #10798 ) ;
#9524 = SURFACE_STYLE_USAGE ( .BOTH. , #13121 ) ;
#9525 = ADVANCED_FACE ( 'NONE', ( #2366 ), #5973, .F. ) ;
#9526 = VERTEX_POINT ( 'NONE', #7057 ) ;
#9527 = AXIS2_PLACEMENT_3D ( 'NONE', #14367, #9829, #6289 ) ;
#9528 = EDGE_LOOP ( 'NONE', ( #14033, #6067, #3335, #7744, #6924, #10864 ) ) ;
#9529 = VERTEX_POINT ( 'NONE', #7133 ) ;
#9530 = ORIENTED_EDGE ( 'NONE', *, *, #2526, .T. ) ;
#9531 = CARTESIAN_POINT ( 'NONE',  ( 2.789999999999999147, -21.30679549418621832, -12.59161484032935618 ) ) ;
#9532 = DIRECTION ( 'NONE',  ( -0.9237280213470682178, -0.3830490080632377725, 0.000000000000000000 ) ) ;
#9533 = CARTESIAN_POINT ( 'NONE',  ( 0.000000000000000000, 0.000000000000000000, 0.000000000000000000 ) ) ;
#9534 = CARTESIAN_POINT ( 'NONE',  ( 1.394999999999999574, -25.12109765559663188, 12.52377138324214378 ) ) ;
#9535 = CARTESIAN_POINT ( 'NONE',  ( 0.5537796532149688034, -3.624349476775314383, 16.55730827443879605 ) ) ;
#9536 = AXIS2_PLACEMENT_3D ( 'NONE', #13322, #13485, #14569 ) ;
#9537 = CIRCLE ( 'NONE', #11006, 6.000000000000000888 ) ;
#9538 = ORIENTED_EDGE ( 'NONE', *, *, #4574, .F. ) ;
#9539 = CARTESIAN_POINT ( 'NONE',  ( 56.98919079003883326, 3.953582723775848962, 7.000000000000000000 ) ) ;
#9540 = B_SPLINE_CURVE_WITH_KNOTS ( 'NONE', 3,
 ( #8607, #9990, #601, #10142, #11215, #689 ),
 .UNSPECIFIED., .F., .F.,
 ( 4, 2, 4 ),
 ( 4.462636732861906317E-07, 0.001879885066975067178, 0.003759323870276848160 ),
 .UNSPECIFIED. ) ;
#9541 = EDGE_CURVE ( 'NONE', #5309, #12675, #2161, .T. ) ;
#9542 = TOROIDAL_SURFACE ( 'NONE', #3902, 24.12539914357697413, 8.000000000000000000 ) ;
#9543 = ORIENTED_EDGE ( 'NONE', *, *, #13952, .F. ) ;
#9544 = CIRCLE ( 'NONE', #8314, 3.000000000000002665 ) ;
#9545 = CARTESIAN_POINT ( 'NONE',  ( 2.718131853594931258, -21.92302674874953539, -12.74240566899008442 ) ) ;
#9546 = CARTESIAN_POINT ( 'NONE',  ( 2.030753616560879493, 24.80264696524883306, 12.05220173035447750 ) ) ;
#9547 = ORIENTED_EDGE ( 'NONE', *, *, #12674, .F. ) ;
#9548 = ORIENTED_EDGE ( 'NONE', *, *, #257, .F. ) ;
#9549 = DIRECTION ( 'NONE',  ( -0.9863939238321437486, -0.1643989873053572359, 0.000000000000000000 ) ) ;
#9550 = EDGE_CURVE ( 'NONE', #6712, #8635, #1443, .T. ) ;
#9551 = EDGE_CURVE ( 'NONE', #4420, #6027, #3339, .T. ) ;
#9552 = ORIENTED_EDGE ( 'NONE', *, *, #9096, .F. ) ;
#9553 = EDGE_CURVE ( 'NONE', #497, #2656, #924, .T. ) ;
#9554 = CARTESIAN_POINT ( 'NONE',  ( 2.789999999999999147, 15.47981323787947794, 0.000000000000000000 ) ) ;
#9555 = CARTESIAN_POINT ( 'NONE',  ( 2.582362678678089107, -15.57879356040261243, -2.899259574942910866 ) ) ;
#9556 = AXIS2_PLACEMENT_3D ( 'NONE', #7863, #12470, #7782 ) ;
#9557 = DIRECTION ( 'NONE',  ( -1.000000000000000000, 0.000000000000000000, -0.000000000000000000 ) ) ;
#9558 = FACE_OUTER_BOUND ( 'NONE', #9838, .T. ) ;
#9559 = ORIENTED_EDGE ( 'NONE', *, *, #4687, .T. ) ;
#9560 = LINE ( 'NONE', #2491, #7444 ) ;
#9561 = DIRECTION ( 'NONE',  ( 0.000000000000000000, 0.000000000000000000, 1.000000000000000000 ) ) ;
#9562 = ORIENTED_EDGE ( 'NONE', *, *, #7788, .T. ) ;
#9563 = CARTESIAN_POINT ( 'NONE',  ( 2.789999999999999591, -24.22479935914660487, 2.133490293296927742 ) ) ;
#9564 = EDGE_LOOP ( 'NONE', ( #14661, #7721, #9374, #14120 ) ) ;
#9565 = ORIENTED_EDGE ( 'NONE', *, *, #2204, .T. ) ;
#9566 = EDGE_CURVE ( 'NONE', #9867, #3792, #3689, .T. ) ;
#9567 = CARTESIAN_POINT ( 'NONE',  ( 0.4522159468065701238, -12.42068120944072795, -11.13074453164216138 ) ) ;
#9568 = VECTOR ( 'NONE', #10891, 1000.000000000000000 ) ;
#9569 = LINE ( 'NONE', #13080, #11485 ) ;
#9570 = ADVANCED_FACE ( 'NONE', ( #8200 ), #112, .T. ) ;
#9571 = CARTESIAN_POINT ( 'NONE',  ( 2.790000000000060876, 14.05326139264727736, 2.096282088614815908 ) ) ;
#9572 = DIRECTION ( 'NONE',  ( -1.000000000000000000, -0.000000000000000000, -0.000000000000000000 ) ) ;
#9573 = DIRECTION ( 'NONE',  ( 0.000000000000000000, 0.000000000000000000, 1.000000000000000000 ) ) ;
#9574 = EDGE_CURVE ( 'NONE', #13626, #1861, #12879, .T. ) ;
#9575 = B_SPLINE_CURVE_WITH_KNOTS ( 'NONE', 3,
 ( #696, #9996, #379, #7690 ),
 .UNSPECIFIED., .F., .F.,
 ( 4, 4 ),
 ( 3.059063720746923042E-07, 0.0006888942284913959508 ),
 .UNSPECIFIED. ) ;
#9576 = CARTESIAN_POINT ( 'NONE',  ( 0.009102498987474663336, -21.10878525316950771, -12.54316204260915768 ) ) ;
#9577 = VERTEX_POINT ( 'NONE', #6131 ) ;
#9578 = CARTESIAN_POINT ( 'NONE',  ( 2.601776121706763423, 19.18368891937490517, 17.47009390565497711 ) ) ;
#9579 = FACE_OUTER_BOUND ( 'NONE', #11348, .T. ) ;
#9580 = CARTESIAN_POINT ( 'NONE',  ( 0.000000000000000000, 0.000000000000000000, -0.8000000000000000444 ) ) ;
#9581 = CARTESIAN_POINT ( 'NONE',  ( 2.765633920072236407, -2.336989772644440855, 24.63872515616082026 ) ) ;
#9582 = EDGE_CURVE ( 'NONE', #8927, #1724, #5913, .T. ) ;
#9583 = ORIENTED_EDGE ( 'NONE', *, *, #5443, .F. ) ;
#9584 = ORIENTED_EDGE ( 'NONE', *, *, #13206, .T. ) ;
#9585 = ORIENTED_EDGE ( 'NONE', *, *, #12009, .F. ) ;
#9586 = CARTESIAN_POINT ( 'NONE',  ( 88.84370878116858705, 10.64188714589527507, 2.999999999999999112 ) ) ;
#9587 = CARTESIAN_POINT ( 'NONE',  ( 14.27437366993929579, -27.03703358530833967, 5.000000000000000000 ) ) ;
#9588 = DIRECTION ( 'NONE',  ( -1.000000000000000000, 0.000000000000000000, -0.000000000000000000 ) ) ;
#9589 = FACE_OUTER_BOUND ( 'NONE', #10114, .T. ) ;
#9590 = DIRECTION ( 'NONE',  ( 1.000000000000000000, 0.000000000000000000, 0.000000000000000000 ) ) ;
#9591 = DIRECTION ( 'NONE',  ( -0.000000000000000000, -0.000000000000000000, -1.000000000000000000 ) ) ;
#9592 = EDGE_LOOP ( 'NONE', ( #9103, #5169, #3295, #4398 ) ) ;
#9593 = DIRECTION ( 'NONE',  ( 0.000000000000000000, 0.000000000000000000, 1.000000000000000000 ) ) ;
#9594 = DIRECTION ( 'NONE',  ( 0.000000000000000000, 0.000000000000000000, 1.000000000000000000 ) ) ;
#9595 = VERTEX_POINT ( 'NONE', #11655 ) ;
#9596 = CARTESIAN_POINT ( 'NONE',  ( -16.96657417111497068, -13.60061260430328467, -3.794707603699265519E-15 ) ) ;
#9597 = CARTESIAN_POINT ( 'NONE',  ( 0.4522159468065704013, 11.13074453164220579, -12.42068120944069420 ) ) ;
#9598 = DIRECTION ( 'NONE',  ( 0.9021244663126475327, 0.4314758942051350465, -1.141265444721583757E-16 ) ) ;
#9599 = VERTEX_POINT ( 'NONE', #13105 ) ;
#9600 = ORIENTED_EDGE ( 'NONE', *, *, #1101, .T. ) ;
#9601 = ORIENTED_EDGE ( 'NONE', *, *, #2510, .T. ) ;
#9602 = VERTEX_POINT ( 'NONE', #14277 ) ;
#9603 = CARTESIAN_POINT ( 'NONE',  ( 0.006974674093432167536, 2.249040938978497994, 24.42374957165206695 ) ) ;
#9604 = DIRECTION ( 'NONE',  ( 1.000000000000000000, 0.000000000000000000, -0.000000000000000000 ) ) ;
#9605 = CARTESIAN_POINT ( 'NONE',  ( 2.790000000000010694, 14.05347802000167512, -2.096460570596210271 ) ) ;
#9606 = FACE_OUTER_BOUND ( 'NONE', #7130, .T. ) ;
#9607 = CARTESIAN_POINT ( 'NONE',  ( 93.34550147531103903, 3.654933296868752457, 2.999999999999999112 ) ) ;
#9608 = DIRECTION ( 'NONE',  ( -1.000000000000000000, -0.000000000000000000, 0.000000000000000000 ) ) ;
#9609 = ADVANCED_FACE ( 'NONE', ( #11804 ), #42, .T. ) ;
#9610 = ORIENTED_EDGE ( 'NONE', *, *, #4222, .T. ) ;
#9611 = CARTESIAN_POINT ( 'NONE',  ( 2.789999999999999147, 19.91106274590514147, 14.18181402625749676 ) ) ;
#9612 = CIRCLE ( 'NONE', #6424, 6.000000000000000888 ) ;
#9613 = ORIENTED_EDGE ( 'NONE', *, *, #10396, .F. ) ;
#9614 = DIRECTION ( 'NONE',  ( 0.000000000000000000, 0.000000000000000000, 1.000000000000000000 ) ) ;
#9615 = EDGE_CURVE ( 'NONE', #15073, #13780, #12931, .T. ) ;
#9616 = DIRECTION ( 'NONE',  ( 1.000000000000000000, 0.000000000000000000, 0.000000000000000000 ) ) ;
#9617 = ORIENTED_EDGE ( 'NONE', *, *, #11882, .T. ) ;
#9618 = ORIENTED_EDGE ( 'NONE', *, *, #12801, .F. ) ;
#9619 = EDGE_CURVE ( 'NONE', #2590, #7147, #9511, .T. ) ;
#9620 = DIRECTION ( 'NONE',  ( 0.000000000000000000, 0.000000000000000000, 1.000000000000000000 ) ) ;
#9621 = ORIENTED_EDGE ( 'NONE', *, *, #10838, .F. ) ;
#9622 = CIRCLE ( 'NONE', #5953, 3.799999999999999378 ) ;
#9623 = AXIS2_PLACEMENT_3D ( 'NONE', #7506, #10806, #1579 ) ;
#9624 = FACE_OUTER_BOUND ( 'NONE', #133, .T. ) ;
#9625 = EDGE_CURVE ( 'NONE', #5508, #14446, #1280, .T. ) ;
#9626 = CARTESIAN_POINT ( 'NONE',  ( 2.789999999999999147, -7.909232158574647009, -21.81711360614308148 ) ) ;
#9627 = CARTESIAN_POINT ( 'NONE',  ( 1.039999999999996261, 24.89775460606850999, -12.96210679857759018 ) ) ;
#9628 = DIRECTION ( 'NONE',  ( -1.000000000000000000, -0.000000000000000000, -0.000000000000000000 ) ) ;
#9629 = VERTEX_POINT ( 'NONE', #3669 ) ;
#9630 = CARTESIAN_POINT ( 'NONE',  ( 2.789999999999999147, 14.46287784598617421, -2.311161484776606212 ) ) ;
#9631 = DIRECTION ( 'NONE',  ( 0.9148936170212765839, 0.4036950204470272086, -0.000000000000000000 ) ) ;
#9632 = ORIENTED_EDGE ( 'NONE', *, *, #14463, .F. ) ;
#9633 = CARTESIAN_POINT ( 'NONE',  ( 0.07473575470096514850, 11.74839219818087521, 9.749517823374048930 ) ) ;
#9634 = EDGE_CURVE ( 'NONE', #3142, #4933, #13193, .T. ) ;
#9635 = ADVANCED_FACE ( 'NONE', ( #7594 ), #4629, .T. ) ;
#9636 = VERTEX_POINT ( 'NONE', #10960 ) ;
#9637 = ORIENTED_EDGE ( 'NONE', *, *, #437, .F. ) ;
#9638 = DIRECTION ( 'NONE',  ( 0.000000000000000000, -1.000000000000000000, 0.000000000000000000 ) ) ;
#9639 = CARTESIAN_POINT ( 'NONE',  ( 2.789999999999999147, -9.324097380959603498, 22.25075486061734864 ) ) ;
#9640 = DIRECTION ( 'NONE',  ( 1.000000000000000000, 0.000000000000000000, 0.000000000000000000 ) ) ;
#9641 = CARTESIAN_POINT ( 'NONE',  ( 2.789999999999999147, 5.249430348645936384, -12.98979500319688718 ) ) ;
#9642 = DIRECTION ( 'NONE',  ( -0.000000000000000000, -0.000000000000000000, -1.000000000000000000 ) ) ;
#9643 = DIRECTION ( 'NONE',  ( -0.9988110320138940956, -0.04874958797097371510, 0.000000000000000000 ) ) ;
#9644 = ORIENTED_EDGE ( 'NONE', *, *, #520, .F. ) ;
#9645 = CARTESIAN_POINT ( 'NONE',  ( 86.00000000000000000, 0.000000000000000000, 7.000000000000000000 ) ) ;
#9646 = CARTESIAN_POINT ( 'NONE',  ( 2.789999999999999147, -13.40591150984231916, 7.739906618939660810 ) ) ;
#9647 = CARTESIAN_POINT ( 'NONE',  ( 0.000000000000000000, -18.28042085475266632, -15.74360496233403239 ) ) ;
#9648 = CARTESIAN_POINT ( 'NONE',  ( -18.40394475573011945, -10.79473832354794460, -5.000000000000000000 ) ) ;
#9649 = EDGE_CURVE ( 'NONE', #12104, #9763, #12106, .T. ) ;
#9650 = EDGE_LOOP ( 'NONE', ( #11767, #9654, #8597, #2545 ) ) ;
#9651 = ORIENTED_EDGE ( 'NONE', *, *, #5364, .T. ) ;
#9652 = EDGE_CURVE ( 'NONE', #13720, #1158, #1315, .T. ) ;
#9653 = EDGE_CURVE ( 'NONE', #12711, #99, #8501, .T. ) ;
#9654 = ORIENTED_EDGE ( 'NONE', *, *, #10095, .T. ) ;
#9655 = LINE ( 'NONE', #9737, #11468 ) ;
#9656 = CARTESIAN_POINT ( 'NONE',  ( 1.749999999999998002, 0.000000000000000000, 0.000000000000000000 ) ) ;
#9657 = DIRECTION ( 'NONE',  ( 0.000000000000000000, 0.000000000000000000, -1.000000000000000000 ) ) ;
#9658 = CARTESIAN_POINT ( 'NONE',  ( 1.039999999999997149, -27.68468304288261805, 4.633866840648821039 ) ) ;
#9659 = CARTESIAN_POINT ( 'NONE',  ( -2.775557561562891351E-14, 0.000000000000000000, 1.395000000000000462 ) ) ;
#9660 = CARTESIAN_POINT ( 'NONE',  ( 1.749999999999998002, 12.96210679857786552, 24.89775460606837143 ) ) ;
#9661 = VERTEX_POINT ( 'NONE', #573 ) ;
#9662 = CARTESIAN_POINT ( 'NONE',  ( 0.7589665203264086557, -19.86422722021297815, -19.12621924769889148 ) ) ;
#9663 = CYLINDRICAL_SURFACE ( 'NONE', #7220, 2.524999999999995914 ) ;
#9664 = ORIENTED_EDGE ( 'NONE', *, *, #8148, .T. ) ;
#9665 = CARTESIAN_POINT ( 'NONE',  ( 1.394999999999999574, 27.76164181293051669, -4.147968289691385202 ) ) ;
#9666 = DIRECTION ( 'NONE',  ( 1.000000000000000000, 0.000000000000000000, 0.000000000000000000 ) ) ;
#9667 = CLOSED_SHELL ( 'NONE', ( #3976, #12651, #1992, #4037, #11219, #1981, #7335, #11684, #7165, #14805, #7109, #6650, #13335, #11367, #13288, #7685, #14155, #10413, #13324, #7428, #6933, #2856, #6523, #14515, #6854, #13295, #14065, #10166, #7199, #13480, #6276, #11254, #234, #14078, #6622, #1407, #4851, #11707, #97, #11787, #9831, #11701, #6433, #12380, #746, #4545, #13615 ) ) ;
#9668 = CYLINDRICAL_SURFACE ( 'NONE', #11639, 3.799999999999999378 ) ;
#9669 = ORIENTED_EDGE ( 'NONE', *, *, #13116, .F. ) ;
#9670 = VECTOR ( 'NONE', #9474, 1000.000000000000000 ) ;
#9671 = CIRCLE ( 'NONE', #12120, 24.12539914357697413 ) ;
#9672 = CARTESIAN_POINT ( 'NONE',  ( 1.749999999999999778, -12.55714665599996138, 12.83329210556827249 ) ) ;
#9673 = B_SPLINE_CURVE_WITH_KNOTS ( 'NONE', 3,
 ( #12263, #3809, #13185, #2810 ),
 .UNSPECIFIED., .F., .F.,
 ( 4, 4 ),
 ( 3.059063720795842371E-07, 0.0006888942284914355242 ),
 .UNSPECIFIED. ) ;
#9674 = B_SPLINE_CURVE_WITH_KNOTS ( 'NONE', 3,
 ( #12584, #12734, #13817, #3289, #10063, #11427 ),
 .UNSPECIFIED., .F., .F.,
 ( 4, 2, 4 ),
 ( 1.979325885420663486E-07, 0.001878588715165612974, 0.003756979497742683576 ),
 .UNSPECIFIED. ) ;
#9675 = CARTESIAN_POINT ( 'NONE',  ( 1.394999999999999574, -12.83329210556840572, 12.55714665599982993 ) ) ;
#9676 = ORIENTED_EDGE ( 'NONE', *, *, #3440, .T. ) ;
#9677 = ORIENTED_EDGE ( 'NONE', *, *, #11225, .T. ) ;
#9678 = ORIENTED_EDGE ( 'NONE', *, *, #14913, .T. ) ;
#9679 = CARTESIAN_POINT ( 'NONE',  ( 0.02531912748631555063, 2.311161484776756758, -14.46287784598614756 ) ) ;
#9680 = CARTESIAN_POINT ( 'NONE',  ( 2.030753602223782206, -27.14986936243577986, 4.828194074574245320 ) ) ;
#9681 = B_SPLINE_CURVE_WITH_KNOTS ( 'NONE', 3,
 ( #5078, #6215, #3915, #2756 ),
 .UNSPECIFIED., .F., .F.,
 ( 4, 4 ),
 ( 0.005258105385878709091, 0.005948373736081389272 ),
 .UNSPECIFIED. ) ;
#9682 = DIRECTION ( 'NONE',  ( 1.000000000000000000, 0.000000000000000000, -0.000000000000000000 ) ) ;
#9683 = CYLINDRICAL_SURFACE ( 'NONE', #6984, 2.999999999999988898 ) ;
#9684 = CARTESIAN_POINT ( 'NONE',  ( -6.115811008765337794E-14, -2.096282088614671579, -14.05326139264730045 ) ) ;
#9685 = AXIS2_PLACEMENT_3D ( 'NONE', #1145, #5541, #9217 ) ;
#9686 = EDGE_CURVE ( 'NONE', #108, #7872, #8278, .T. ) ;
#9687 = VECTOR ( 'NONE', #8633, 1000.000000000000114 ) ;
#9689 = AXIS2_PLACEMENT_3D ( 'NONE', #5003, #11892, #10674 ) ;
#9688 = DIRECTION ( 'NONE',  ( 1.000000000000000000, 0.000000000000000000, 0.000000000000000000 ) ) ;
#9690 =( REPRESENTATION_RELATIONSHIP ('NONE','NONE', #12685, #7891 ) REPRESENTATION_RELATIONSHIP_WITH_TRANSFORMATION ( #7355 )SHAPE_REPRESENTATION_RELATIONSHIP( ) );
#9691 = ORIENTED_EDGE ( 'NONE', *, *, #13890, .F. ) ;
#9692 = DIRECTION ( 'NONE',  ( 0.000000000000000000, 0.000000000000000000, 1.000000000000000000 ) ) ;
#9693 = TOROIDAL_SURFACE ( 'NONE', #12139, 14.01039946648073986, 8.000000000000000000 ) ;
#9694 = TOROIDAL_SURFACE ( 'NONE', #5530, 24.12539914357697768, 8.000000000000000000 ) ;
#9695 = CIRCLE ( 'NONE', #3079, 4.000000000000000000 ) ;
#9696 = VERTEX_POINT ( 'NONE', #12032 ) ;
#9697 = ORIENTED_EDGE ( 'NONE', *, *, #8412, .F. ) ;
#9698 = DIRECTION ( 'NONE',  ( 0.000000000000000000, 6.870191984066563922E-16, -1.000000000000000000 ) ) ;
#9699 = CARTESIAN_POINT ( 'NONE',  ( 1.749999999999998002, 25.12109765559653596, 12.52377138324232675 ) ) ;
#9700 = EDGE_CURVE ( 'NONE', #13976, #2534, #5602, .T. ) ;
#9701 = ORIENTED_EDGE ( 'NONE', *, *, #11745, .T. ) ;
#9702 = LINE ( 'NONE', #7478, #9958 ) ;
#9703 = AXIS2_PLACEMENT_3D ( 'NONE', #2736, #2883, #5132 ) ;
#9704 = ORIENTED_EDGE ( 'NONE', *, *, #14809, .F. ) ;
#9705 = AXIS2_PLACEMENT_3D ( 'NONE', #1862, #5414, #11001 ) ;
#9706 = FACE_OUTER_BOUND ( 'NONE', #5655, .T. ) ;
#9707 = DIRECTION ( 'NONE',  ( 1.000000000000000000, 0.000000000000000000, 0.000000000000000000 ) ) ;
#9708 = ADVANCED_FACE ( 'NONE', ( #4137 ), #1919, .T. ) ;
#9709 = CARTESIAN_POINT ( 'NONE',  ( -1.149999999999998135, 0.000000000000000000, -4.000000000000000000 ) ) ;
#9710 = ORIENTED_EDGE ( 'NONE', *, *, #2884, .T. ) ;
#9711 = CARTESIAN_POINT ( 'NONE',  ( 0.7589665283900990378, 3.797536611356696845, -27.31260702007171304 ) ) ;
#9712 = EDGE_CURVE ( 'NONE', #3345, #2360, #6826, .T. ) ;
#9713 = CARTESIAN_POINT ( 'NONE',  ( 0.2818302809372413287, 12.18203740414281278, -10.58084377126610498 ) ) ;
#9714 = ORIENTED_EDGE ( 'NONE', *, *, #5817, .F. ) ;
#9715 = LINE ( 'NONE', #14412, #5338 ) ;
#9716 = TOROIDAL_SURFACE ( 'NONE', #11670, 24.12539914357697413, 8.000000000000000000 ) ;
#9717 = LINE ( 'NONE', #14119, #9687 ) ;
#9718 = ORIENTED_EDGE ( 'NONE', *, *, #11813, .T. ) ;
#9719 = EDGE_LOOP ( 'NONE', ( #11332, #7504, #13046, #1117 ) ) ;
#9720 = CARTESIAN_POINT ( 'NONE',  ( 2.790000000000077307, -9.515416771311352662, 22.38018801136472646 ) ) ;
#9721 = DIRECTION ( 'NONE',  ( 1.000000000000000000, 0.000000000000000000, 0.000000000000000000 ) ) ;
#9722 = DIRECTION ( 'NONE',  ( -1.000000000000000000, 0.000000000000000000, -0.000000000000000000 ) ) ;
#9723 = ITEM_DEFINED_TRANSFORMATION ( 'NONE', 'NONE', #13081,  #1376 ) ;
#9724 = CIRCLE ( 'NONE', #2606, 2.524999999999995914 ) ;
#9725 = DIRECTION ( 'NONE',  ( -1.000000000000000000, -0.000000000000000000, -0.000000000000000000 ) ) ;
#9726 = EDGE_LOOP ( 'NONE', ( #13992, #13377, #7293, #106, #4558, #1262 ) ) ;
#9727 = FACE_OUTER_BOUND ( 'NONE', #6647, .T. ) ;
#9728 = CARTESIAN_POINT ( 'NONE',  ( -16.64001273322991281, -13.79473832354794993, 14.99999999999999822 ) ) ;
#9729 = DIRECTION ( 'NONE',  ( 1.000000000000000000, 0.000000000000000000, 0.000000000000000000 ) ) ;
#9730 = CARTESIAN_POINT ( 'NONE',  ( 0.000000000000000000, 24.34211360614300190, 7.909232158574900140 ) ) ;
#9731 = VERTEX_POINT ( 'NONE', #6279 ) ;
#9732 = ORIENTED_EDGE ( 'NONE', *, *, #12360, .T. ) ;
#9733 = COLOUR_RGB ( '',0.8941176470588234615, 0.8941176470588234615, 0.8941176470588234615 ) ;
#9734 = CIRCLE ( 'NONE', #7544, 3.799999999999999378 ) ;
#9735 = ADVANCED_FACE ( 'NONE', ( #9738 ), #8813, .T. ) ;
#9736 = ORIENTED_EDGE ( 'NONE', *, *, #5488, .T. ) ;
#9737 = CARTESIAN_POINT ( 'NONE',  ( 1.394999999999998685, 25.12109765559653596, 12.52377138324232675 ) ) ;
#9738 = FACE_OUTER_BOUND ( 'NONE', #928, .T. ) ;
#9739 = AXIS2_PLACEMENT_3D ( 'NONE', #14062, #861, #14297 ) ;
#9740 = CARTESIAN_POINT ( 'NONE',  ( -18.40394475573011945, -10.79473832354794460, -5.000000000000000000 ) ) ;
#9741 = DIRECTION ( 'NONE',  ( -1.445602896647338917E-16, 1.000000000000000000, -0.000000000000000000 ) ) ;
#9742 = DIRECTION ( 'NONE',  ( 1.000000000000000000, 0.000000000000000000, 0.000000000000000000 ) ) ;
#9743 = CIRCLE ( 'NONE', #3605, 4.000000000000000000 ) ;
#9744 = CARTESIAN_POINT ( 'NONE',  ( 2.646101151981377075, 14.59528211759998406, 5.279841123860917307 ) ) ;
#9745 = ORIENTED_EDGE ( 'NONE', *, *, #12093, .F. ) ;
#9746 = DIRECTION ( 'NONE',  ( -0.4036950204470267645, 0.9148936170212766950, 0.000000000000000000 ) ) ;
#9747 = DIRECTION ( 'NONE',  ( 0.000000000000000000, 0.000000000000000000, 1.000000000000000000 ) ) ;
#9748 = EDGE_CURVE ( 'NONE', #613, #12163, #7811, .T. ) ;
#9749 = ADVANCED_FACE ( 'NONE', ( #9883 ), #1815, .F. ) ;
#9750 = ORIENTED_EDGE ( 'NONE', *, *, #8360, .T. ) ;
#9752 = AXIS2_PLACEMENT_3D ( 'NONE', #10109, #4203, #4352 ) ;
#9751 = LINE ( 'NONE', #585, #6828 ) ;
#9753 = CARTESIAN_POINT ( 'NONE',  ( -3.751931928061364552, 0.6025004624012588739, 6.999999999999989342 ) ) ;
#9754 = DIRECTION ( 'NONE',  ( 1.576560579138138762E-17, -1.359337748750801608E-17, 1.000000000000000000 ) ) ;
#9755 = ORIENTED_EDGE ( 'NONE', *, *, #2735, .T. ) ;
#9756 = AXIS2_PLACEMENT_3D ( 'NONE', #10658, #9510, #8351 ) ;
#9757 = VECTOR ( 'NONE', #10050, 1000.000000000000114 ) ;
#9758 = CARTESIAN_POINT ( 'NONE',  ( 1.885839517048297775, 17.20101185193998816, -4.239993951493249646 ) ) ;
#9760 = TOROIDAL_SURFACE ( 'NONE', #5358, 5.899999999999999467, 0.1000000000000010186 ) ;
#9759 = LINE ( 'NONE', #9675, #2353 ) ;
#9761 = VERTEX_POINT ( 'NONE', #8652 ) ;
#9762 = VERTEX_POINT ( 'NONE', #2819 ) ;
#9763 = VERTEX_POINT ( 'NONE', #12190 ) ;
#9764 = CARTESIAN_POINT ( 'NONE',  ( 2.765633920072241736, -9.836394144775550075, -22.71065055754462492 ) ) ;
#9765 = CARTESIAN_POINT ( 'NONE',  ( 0.000000000000000000, 0.000000000000000000, 0.000000000000000000 ) ) ;
#9766 = CARTESIAN_POINT ( 'NONE',  ( -7.646929282184496191E-14, 5.456611084822186264, -23.69897269326672884 ) ) ;
#9767 = DIRECTION ( 'NONE',  ( 1.000000000000000000, 0.000000000000000000, 0.000000000000000000 ) ) ;
#9768 = EDGE_CURVE ( 'NONE', #1826, #7052, #12698, .T. ) ;
#9769 = DIRECTION ( 'NONE',  ( 0.000000000000000000, 0.000000000000000000, -1.000000000000000000 ) ) ;
#9770 = ADVANCED_FACE ( 'NONE', ( #14583 ), #4054, .F. ) ;
#9771 = AXIS2_PLACEMENT_3D ( 'NONE', #8636, #11096, #7264 ) ;
#9772 = DIRECTION ( 'NONE',  ( -1.000000000000000000, 0.000000000000000000, 0.000000000000000000 ) ) ;
#9773 = ADVANCED_FACE ( 'NONE', ( #6427 ), #11110, .T. ) ;
#9774 = VERTEX_POINT ( 'NONE', #12419 ) ;
#9775 = LINE ( 'NONE', #8612, #12900 ) ;
#9776 = CIRCLE ( 'NONE', #12701, 2.447112362156698140 ) ;
#9777 = EDGE_CURVE ( 'NONE', #5623, #2515, #14888, .T. ) ;
#9778 =( LENGTH_UNIT ( ) NAMED_UNIT ( * ) SI_UNIT ( .MILLI., .METRE. ) );
#9779 = ORIENTED_EDGE ( 'NONE', *, *, #8584, .F. ) ;
#9780 = ORIENTED_EDGE ( 'NONE', *, *, #5389, .T. ) ;
#9781 = CARTESIAN_POINT ( 'NONE',  ( -6.202591138825049061E-14, 8.842064619038524143, 11.12234047011193283 ) ) ;
#9782 = CARTESIAN_POINT ( 'NONE',  ( 2.789999999999999147, 1.948757464274366136, -13.87420763704359139 ) ) ;
#9783 = ORIENTED_EDGE ( 'NONE', *, *, #10498, .T. ) ;
#9784 = CIRCLE ( 'NONE', #9536, 4.100000000000000533 ) ;
#9785 = AXIS2_PLACEMENT_3D ( 'NONE', #5285, #10948, #14506 ) ;
#9786 = PRODUCT_DEFINITION_CONTEXT ( 'detailed design', #7547, 'design' ) ;
#9787 = CARTESIAN_POINT ( 'NONE',  ( 1.394999999999998685, -4.147968289691093879, -27.76164181293055933 ) ) ;
#9788 = B_SPLINE_CURVE_WITH_KNOTS ( 'NONE', 3,
 ( #10252, #14954, #4651, #9251 ),
 .UNSPECIFIED., .F., .F.,
 ( 4, 4 ),
 ( 0.005123695899043906321, 0.005814329666474870977 ),
 .UNSPECIFIED. ) ;
#9789 = EDGE_LOOP ( 'NONE', ( #11095, #1006 ) ) ;
#9790 = CARTESIAN_POINT ( 'NONE',  ( 1.387778780781445676E-14, 0.000000000000000000, -7.000000000000007994 ) ) ;
#9791 = CARTESIAN_POINT ( 'NONE',  ( 2.789999999999999147, -22.25075486061744812, 9.324097380959361914 ) ) ;
#9792 = CARTESIAN_POINT ( 'NONE',  ( 91.46153288930040048, 16.46030115554384565, 2.999999999999999112 ) ) ;
#9793 = AXIS2_PLACEMENT_3D ( 'NONE', #1507, #10951, #6196 ) ;
#9794 = AXIS2_PLACEMENT_3D ( 'NONE', #3336, #8024, #12706 ) ;
#9795 = AXIS2_PLACEMENT_3D ( 'NONE', #1750, #7825, #10053 ) ;
#9796 = CARTESIAN_POINT ( 'NONE',  ( -9.999999999999992895, -25.00000000000000000, -130.1575142076926852 ) ) ;
#9797 = CARTESIAN_POINT ( 'NONE',  ( 1.039999999999997593, 0.000000000000000000, 0.000000000000000000 ) ) ;
#9798 = ORIENTED_EDGE ( 'NONE', *, *, #3715, .T. ) ;
#9799 = CARTESIAN_POINT ( 'NONE',  ( 0.006931038682726457442, 12.53626894672828485, 21.08061549536619950 ) ) ;
#9800 = EDGE_LOOP ( 'NONE', ( #7927, #13170, #2460, #12259 ) ) ;
#9801 = ORIENTED_EDGE ( 'NONE', *, *, #13027, .T. ) ;
#9802 = CARTESIAN_POINT ( 'NONE',  ( 1.150000000000000577, 0.000000000000000000, -5.899999999999999467 ) ) ;
#9803 = DIRECTION ( 'NONE',  ( 1.000000000000000000, 0.000000000000000000, -0.000000000000000000 ) ) ;
#9804 = SHAPE_REPRESENTATION_RELATIONSHIP ( 'NONE' , 'NONE' ,  #1017, #14434 ) ;
#9805 = CARTESIAN_POINT ( 'NONE',  ( 80.82762530298222714, -19.99999999999999645, 3.000000000000002665 ) ) ;
#9806 = AXIS2_PLACEMENT_3D ( 'NONE', #1012, #10384, #15081 ) ;
#9807 = CARTESIAN_POINT ( 'NONE',  ( -5.209999999999999964, 0.000000000000000000, 0.000000000000000000 ) ) ;
#9808 = VERTEX_POINT ( 'NONE', #886 ) ;
#9809 = CARTESIAN_POINT ( 'NONE',  ( 67.23404255319145761, 28.93147646537025963, -8.169391093593850073 ) ) ;
#9810 = CARTESIAN_POINT ( 'NONE',  ( 2.764680872515354881, -13.68080036884352246, 5.229914364928304416 ) ) ;
#9811 = CARTESIAN_POINT ( 'NONE',  ( 2.789999999999999147, -5.391175441198789109, 24.15498966839961170 ) ) ;
#9812 = CYLINDRICAL_SURFACE ( 'NONE', #8514, 8.400000000000000355 ) ;
#9813 = VERTEX_POINT ( 'NONE', #3047 ) ;
#9814 = CIRCLE ( 'NONE', #2214, 0.5999999999999999778 ) ;
#9815 = ORIENTED_EDGE ( 'NONE', *, *, #2409, .T. ) ;
#9816 = B_SPLINE_CURVE_WITH_KNOTS ( 'NONE', 3,
 ( #3160, #10216, #10071, #7845 ),
 .UNSPECIFIED., .F., .F.,
 ( 4, 4 ),
 ( 1.981826382900813409E-07, 0.0006887856082032186092 ),
 .UNSPECIFIED. ) ;
#9817 = ORIENTED_EDGE ( 'NONE', *, *, #15097, .F. ) ;
#9818 = CARTESIAN_POINT ( 'NONE',  ( 0.000000000000000000, 12.98979500319701685, -5.249430348645618416 ) ) ;
#9819 = CARTESIAN_POINT ( 'NONE',  ( -1.000000000000000000, -5.408326913195983465, -0.8000000000000000444 ) ) ;
#9820 = DIRECTION ( 'NONE',  ( -1.000000000000000000, 0.000000000000000000, 0.000000000000000000 ) ) ;
#9821 = CARTESIAN_POINT ( 'NONE',  ( 0.000000000000000000, 0.000000000000000000, 0.000000000000000000 ) ) ;
#9822 = SHAPE_DEFINITION_REPRESENTATION ( #256, #4172 ) ;
#9823 = LINE ( 'NONE', #12195, #12073 ) ;
#9824 = ADVANCED_FACE ( 'NONE', ( #2203 ), #681, .T. ) ;
#9825 = VERTEX_POINT ( 'NONE', #6664 ) ;
#9826 = PLANE ( 'NONE',  #6873 ) ;
#9827 = DIRECTION ( 'NONE',  ( -1.000000000000000000, -0.000000000000000000, -0.000000000000000000 ) ) ;
#9828 = ORIENTED_EDGE ( 'NONE', *, *, #8353, .T. ) ;
#9829 = DIRECTION ( 'NONE',  ( 0.000000000000000000, 0.000000000000000000, 1.000000000000000000 ) ) ;
#9830 = CARTESIAN_POINT ( 'NONE',  ( 1.394999999999998685, 4.458161950358745074, -17.39253030560836777 ) ) ;
#9831 = ADVANCED_FACE ( 'NONE', ( #12641 ), #4439, .F. ) ;
#9832 = DIRECTION ( 'NONE',  ( 1.000000000000000000, 0.000000000000000000, 0.000000000000000000 ) ) ;
#9833 = ORIENTED_EDGE ( 'NONE', *, *, #5415, .F. ) ;
#9834 = CYLINDRICAL_SURFACE ( 'NONE', #11915, 2.524999999999995914 ) ;
#9835 = CARTESIAN_POINT ( 'NONE',  ( -9.999999999999998224, -1.390791565672605534, -130.1575142076926852 ) ) ;
#9836 = EDGE_LOOP ( 'NONE', ( #6266, #10919, #14523, #6986 ) ) ;
#9837 = ORIENTED_EDGE ( 'NONE', *, *, #9934, .F. ) ;
#9838 = EDGE_LOOP ( 'NONE', ( #10590, #8860, #6964, #4128 ) ) ;
#9839 = DIRECTION ( 'NONE',  ( 1.000000000000000000, 0.000000000000000000, 0.000000000000000000 ) ) ;
#9840 = ADVANCED_FACE ( 'NONE', ( #9122 ), #13801, .T. ) ;
#9841 = EDGE_CURVE ( 'NONE', #12348, #9402, #10116, .T. ) ;
#9842 = CARTESIAN_POINT ( 'NONE',  ( 2.031033479673589159, 19.12621924769867121, 19.86422722021319487 ) ) ;
#9843 = CARTESIAN_POINT ( 'NONE',  ( 1.749999999999998002, 0.000000000000000000, 0.000000000000000000 ) ) ;
#9844 = CARTESIAN_POINT ( 'NONE',  ( 2.789999999999999147, 1.621424371464993087E-13, -12.95481323787947936 ) ) ;
#9845 = CARTESIAN_POINT ( 'NONE',  ( 0.000000000000000000, 20.62201879784932856, -12.52067188844328705 ) ) ;
#9846 = ORIENTED_EDGE ( 'NONE', *, *, #10396, .T. ) ;
#9847 = DIRECTION ( 'NONE',  ( -1.000000000000000000, -0.000000000000000000, -0.000000000000000000 ) ) ;
#9848 = ADVANCED_FACE ( 'NONE', ( #745 ), #10193, .T. ) ;
#9849 = VERTEX_POINT ( 'NONE', #7894 ) ;
#9850 = ORIENTED_EDGE ( 'NONE', *, *, #8983, .F. ) ;
#9851 = CARTESIAN_POINT ( 'NONE',  ( 0.1999999999999985678, -6.997142273814360713, 0.000000000000000000 ) ) ;
#9852 = DIRECTION ( 'NONE',  ( -1.000000000000000000, -0.000000000000000000, -0.000000000000000000 ) ) ;
#9853 = ADVANCED_FACE ( 'NONE', ( #7820 ), #13876, .T. ) ;
#9854 = ORIENTED_EDGE ( 'NONE', *, *, #7297, .F. ) ;
#9855 = CYLINDRICAL_SURFACE ( 'NONE', #14388, 4.000000000000003553 ) ;
#9856 = ADVANCED_FACE ( 'NONE', ( #14813 ), #14744, .F. ) ;
#9857 = VERTEX_POINT ( 'NONE', #10340 ) ;
#9858 = CARTESIAN_POINT ( 'NONE',  ( 1.749999999999999778, 12.83329210556831690, 12.55714665599991875 ) ) ;
#9859 = CARTESIAN_POINT ( 'NONE',  ( 101.6227766016837819, -9.999999999999994671, -130.1575142076926852 ) ) ;
#9860 = CARTESIAN_POINT ( 'NONE',  ( 2.765633920072239516, 16.37294372382858398, 18.55949924794898465 ) ) ;
#9861 = CARTESIAN_POINT ( 'NONE',  ( 0.000000000000000000, 23.48180575137739368, -5.535312321042471062 ) ) ;
#9862 = FACE_OUTER_BOUND ( 'NONE', #13394, .T. ) ;
#9863 = ORIENTED_EDGE ( 'NONE', *, *, #6293, .F. ) ;
#9864 = CARTESIAN_POINT ( 'NONE',  ( 2.459751808031945922E-16, 12.51294990530016271, 20.85230829256858343 ) ) ;
#9865 = CARTESIAN_POINT ( 'NONE',  ( 2.789999999999999147, 2.336989772644269436, 24.63872515616083447 ) ) ;
#9866 = ORIENTED_EDGE ( 'NONE', *, *, #3200, .F. ) ;
#9867 = VERTEX_POINT ( 'NONE', #8881 ) ;
#9868 = FACE_OUTER_BOUND ( 'NONE', #11489, .T. ) ;
#9869 = FACE_OUTER_BOUND ( 'NONE', #1753, .T. ) ;
#9870 = AXIS2_PLACEMENT_3D ( 'NONE', #9646, #11945, #6419 ) ;
#9871 = CARTESIAN_POINT ( 'NONE',  ( -1.250000000000001110, 0.000000000000000000, 0.000000000000000000 ) ) ;
#9872 = EDGE_CURVE ( 'NONE', #13954, #1071, #10263, .T. ) ;
#9873 = ORIENTED_EDGE ( 'NONE', *, *, #7156, .F. ) ;
#9874 = DIRECTION ( 'NONE',  ( 2.081668171172168513E-16, -1.000000000000000000, 0.000000000000000000 ) ) ;
#9875 = CARTESIAN_POINT ( 'NONE',  ( 91.12964445316929130, 15.08873975234342701, 7.000000000000000000 ) ) ;
#9876 = DIRECTION ( 'NONE',  ( 0.000000000000000000, 0.000000000000000000, 1.000000000000000000 ) ) ;
#9877 = CARTESIAN_POINT ( 'NONE',  ( 0.000000000000000000, 0.000000000000000000, 0.000000000000000000 ) ) ;
#9878 = AXIS2_PLACEMENT_3D ( 'NONE', #10444, #9431, #6981 ) ;
#9879 = ORIENTED_EDGE ( 'NONE', *, *, #13416, .T. ) ;
#9880 = ORIENTED_EDGE ( 'NONE', *, *, #11826, .F. ) ;
#9881 = ORIENTED_EDGE ( 'NONE', *, *, #5143, .F. ) ;
#9882 = CARTESIAN_POINT ( 'NONE',  ( 0.02436607992776498519, -21.30679549418621832, -12.59161484032935618 ) ) ;
#9883 = FACE_OUTER_BOUND ( 'NONE', #2648, .T. ) ;
#9884 = EDGE_CURVE ( 'NONE', #8779, #15019, #14940, .T. ) ;
#9885 = CARTESIAN_POINT ( 'NONE',  ( 2.718131864678289933, -2.577209017046833583, -25.22589920183363787 ) ) ;
#9886 = CARTESIAN_POINT ( 'NONE',  ( 2.718184743034447681, -5.344212458769196594, -24.78695292654926519 ) ) ;
#9887 = SHAPE_DEFINITION_REPRESENTATION ( #11545, #5737 ) ;
#9888 = CARTESIAN_POINT ( 'NONE',  ( 2.715264182578264851, 5.299647274067300629, -14.31752701692930962 ) ) ;
#9889 = CYLINDRICAL_SURFACE ( 'NONE', #3677, 17.95481323787947403 ) ;
#9890 = CARTESIAN_POINT ( 'NONE',  ( 1.749999999999998002, 25.12109765559671004, -12.52377138324198391 ) ) ;
#9891 = ORIENTED_EDGE ( 'NONE', *, *, #8428, .T. ) ;
#9892 = CARTESIAN_POINT ( 'NONE',  ( 72.49759028996473376, 17.18292470770558822, 4.000000000000000000 ) ) ;
#9893 = CARTESIAN_POINT ( 'NONE',  ( 5.999999999999999112, 7.347880794884118750E-16, 3.895000000000000462 ) ) ;
#9894 = LINE ( 'NONE', #6371, #7724 ) ;
#9895 = EDGE_CURVE ( 'NONE', #5963, #6156, #10272, .T. ) ;
#9896 = ORIENTED_EDGE ( 'NONE', *, *, #6234, .T. ) ;
#9897 = EDGE_CURVE ( 'NONE', #5629, #5631, #14201, .T. ) ;
#9898 = LINE ( 'NONE', #14599, #12903 ) ;
#9899 = CARTESIAN_POINT ( 'NONE',  ( 1.039999999999998925, -4.147968289691484678, 27.76164181293050248 ) ) ;
#9900 = ORIENTED_EDGE ( 'NONE', *, *, #11578, .T. ) ;
#9901 = ORIENTED_EDGE ( 'NONE', *, *, #8253, .F. ) ;
#9902 = CYLINDRICAL_SURFACE ( 'NONE', #6551, 4.000000000000003553 ) ;
#9903 = DIRECTION ( 'NONE',  ( 1.000000000000000000, -0.000000000000000000, -0.000000000000000000 ) ) ;
#9904 = CARTESIAN_POINT ( 'NONE',  ( 88.84370878116860126, 10.64188714589527684, 6.000000000000000000 ) ) ;
#9905 = CARTESIAN_POINT ( 'NONE',  ( -19.40394475573011590, -4.794738323547945491, 22.00000000000000000 ) ) ;
#9906 = DIRECTION ( 'NONE',  ( -0.000000000000000000, -0.000000000000000000, -1.000000000000000000 ) ) ;
#9907 = TOROIDAL_SURFACE ( 'NONE', #12003, 24.12539914357697413, 8.000000000000000000 ) ;
#9908 = CLOSED_SHELL ( 'NONE', ( #7606, #11868, #7973, #6733, #4506, #7576, #7110, #2459, #455, #694, #1304, #6710, #2782, #4080, #5786, #11308, #4331, #2897, #9824, #12071, #10885, #3650, #6640, #6116, #13548, #9023, #12692, #7329 ) ) ;
#9909 = DIRECTION ( 'NONE',  ( -1.000000000000000000, -0.000000000000000000, -0.000000000000000000 ) ) ;
#9910 = ORIENTED_EDGE ( 'NONE', *, *, #9288, .T. ) ;
#9911 = CARTESIAN_POINT ( 'NONE',  ( 2.790000000000076419, -2.133839912090968127, 24.22524813288760726 ) ) ;
#9912 = CARTESIAN_POINT ( 'NONE',  ( 18.87754531448929995, -24.24225080111726527, 7.000000000000000000 ) ) ;
#9913 = ADVANCED_FACE ( 'NONE', ( #9191 ), #6731, .T. ) ;
#9914 = AXIS2_PLACEMENT_3D ( 'NONE', #7209, #11885, #13038 ) ;
#9915 = ORIENTED_EDGE ( 'NONE', *, *, #12938, .T. ) ;
#9916 = ORIENTED_EDGE ( 'NONE', *, *, #10840, .T. ) ;
#9917 = ORIENTED_EDGE ( 'NONE', *, *, #3737, .F. ) ;
#9918 = DIRECTION ( 'NONE',  ( -1.000000000000000000, 0.000000000000000000, 0.000000000000000000 ) ) ;
#9919 = AXIS2_PLACEMENT_3D ( 'NONE', #13133, #3844, #10908 ) ;
#9920 = CARTESIAN_POINT ( 'NONE',  ( 1.566204647097437341, -6.822536405429464601, -0.8000000000000000444 ) ) ;
#9921 = ORIENTED_EDGE ( 'NONE', *, *, #2996, .F. ) ;
#9922 = AXIS2_PLACEMENT_3D ( 'NONE', #13291, #8608, #2771 ) ;
#9923 = EDGE_CURVE ( 'NONE', #1158, #12816, #11636, .T. ) ;
#9924 = VECTOR ( 'NONE', #1073, 1000.000000000000000 ) ;
#9925 = UNCERTAINTY_MEASURE_WITH_UNIT (LENGTH_MEASURE( 1.000000000000000082E-05 ), #4169, 'distance_accuracy_value', 'NONE');
#9926 = DIRECTION ( 'NONE',  ( 0.000000000000000000, 0.000000000000000000, 1.000000000000000000 ) ) ;
#9927 = FACE_OUTER_BOUND ( 'NONE', #13333, .T. ) ;
#9928 = ORIENTED_EDGE ( 'NONE', *, *, #4776, .F. ) ;
#9929 = FACE_OUTER_BOUND ( 'NONE', #14546, .T. ) ;
#9930 = CARTESIAN_POINT ( 'NONE',  ( -6.403158385254602634E-17, -23.69843731927173991, 5.456805104201007950 ) ) ;
#9931 = VECTOR ( 'NONE', #8043, 1000.000000000000000 ) ;
#9932 = EDGE_CURVE ( 'NONE', #9447, #1296, #9569, .T. ) ;
#9933 = VECTOR ( 'NONE', #4181, 1000.000000000000114 ) ;
#9934 = EDGE_CURVE ( 'NONE', #6218, #10191, #12671, .T. ) ;
#9935 = CARTESIAN_POINT ( 'NONE',  ( 0.07186808533286645484, -10.24630254990532663, 23.19485392143210944 ) ) ;
#9936 = VECTOR ( 'NONE', #5357, 1000.000000000000000 ) ;
#9937 = DIRECTION ( 'NONE',  ( 0.000000000000000000, 0.000000000000000000, -1.000000000000000000 ) ) ;
#9938 = CARTESIAN_POINT ( 'NONE',  ( 0.006931111373680289185, 9.685942809247373830, -22.53293026234493723 ) ) ;
#9939 = EDGE_LOOP ( 'NONE', ( #10712, #10112, #5701, #473, #3082, #1189, #1345, #4447 ) ) ;
#9940 = CARTESIAN_POINT ( 'NONE',  ( 1.749999999999999778, 0.000000000000000000, 0.000000000000000000 ) ) ;
#9941 = CARTESIAN_POINT ( 'NONE',  ( 2.246812931352479392, -12.54666350726115631, -11.42270873787306229 ) ) ;
#9942 = VERTEX_POINT ( 'NONE', #2497 ) ;
#9943 = ORIENTED_EDGE ( 'NONE', *, *, #6507, .T. ) ;
#9944 = CARTESIAN_POINT ( 'NONE',  ( 0.000000000000000000, 5.249430348645932831, -12.98979500319689251 ) ) ;
#9946 = FACE_BOUND ( 'NONE', #1452, .T. ) ;
#9945 = VECTOR ( 'NONE', #11253, 1000.000000000000000 ) ;
#9947 = VECTOR ( 'NONE', #5416, 1000.000000000000227 ) ;
#9948 = FILL_AREA_STYLE_COLOUR ( '', #1658 ) ;
#9949 = DIRECTION ( 'NONE',  ( 0.000000000000000000, 0.000000000000000000, -1.000000000000000000 ) ) ;
#9950 = EDGE_CURVE ( 'NONE', #10680, #7949, #944, .T. ) ;
#9951 = EDGE_CURVE ( 'NONE', #7072, #12029, #14185, .T. ) ;
#9952 = CARTESIAN_POINT ( 'NONE',  ( 2.789999999999999147, -1.948757464274075479, -13.87420763704363225 ) ) ;
#9954 = ORIENTED_EDGE ( 'NONE', *, *, #752, .T. ) ;
#9953 = EDGE_CURVE ( 'NONE', #6110, #8350, #11786, .T. ) ;
#9955 = CARTESIAN_POINT ( 'NONE',  ( 2.789999999999999147, -24.44424927289185590, -0.2301004812060095106 ) ) ;
#9956 = DIRECTION ( 'NONE',  ( -1.000000000000000000, -0.000000000000000000, -0.000000000000000000 ) ) ;
#9957 = VERTEX_POINT ( 'NONE', #2273 ) ;
#9958 = VECTOR ( 'NONE', #8461, 1000.000000000000000 ) ;
#9959 = FILL_AREA_STYLE_COLOUR ( '', #9733 ) ;
#9960 = CIRCLE ( 'NONE', #3333, 2.999999999999988898 ) ;
#9961 = ORIENTED_EDGE ( 'NONE', *, *, #5649, .T. ) ;
#9962 = ORIENTED_EDGE ( 'NONE', *, *, #340, .T. ) ;
#9963 = EDGE_CURVE ( 'NONE', #9387, #9402, #14026, .T. ) ;
#9964 = ORIENTED_EDGE ( 'NONE', *, *, #6159, .T. ) ;
#9965 = CARTESIAN_POINT ( 'NONE',  ( 0.1882238946918228795, -25.78859396478530641, 2.857713464478602194 ) ) ;
#9966 = CARTESIAN_POINT ( 'NONE',  ( 0.1855654851361735469, 10.67816411292198175, -23.63475234378971379 ) ) ;
#9967 = LINE ( 'NONE', #2974, #667 ) ;
#9968 = DIRECTION ( 'NONE',  ( 1.000000000000000000, -0.000000000000000000, 0.000000000000000000 ) ) ;
#9969 = CARTESIAN_POINT ( 'NONE',  ( 0.000000000000000000, 0.000000000000000000, 0.000000000000000000 ) ) ;
#9970 = CARTESIAN_POINT ( 'NONE',  ( 2.783025325906568259, 24.42374957165205629, 2.249040938978581927 ) ) ;
#9971 = CIRCLE ( 'NONE', #13896, 28.06981291497571362 ) ;
#9972 = AXIS2_PLACEMENT_3D ( 'NONE', #5447, #10118, #14889 ) ;
#9973 = CARTESIAN_POINT ( 'NONE',  ( 0.7589665326895898012, 24.32849926382769468, -12.98167595240995986 ) ) ;
#9974 = DIRECTION ( 'NONE',  ( 1.000000000000000000, 0.000000000000000000, -0.000000000000000000 ) ) ;
#9975 = VERTEX_POINT ( 'NONE', #8335 ) ;
#9976 = DIRECTION ( 'NONE',  ( -0.000000000000000000, -0.000000000000000000, -1.000000000000000000 ) ) ;
#9977 = CARTESIAN_POINT ( 'NONE',  ( 2.718184743034448569, 24.78695292654929005, -5.344212458769106888 ) ) ;
#9978 = CIRCLE ( 'NONE', #3349, 28.06981291497571362 ) ;
#9979 = VERTEX_POINT ( 'NONE', #10415 ) ;
#9980 = VECTOR ( 'NONE', #12159, 1000.000000000000114 ) ;
#9981 = LINE ( 'NONE', #285, #8248 ) ;
#9982 = DIRECTION ( 'NONE',  ( -0.000000000000000000, -0.000000000000000000, -1.000000000000000000 ) ) ;
#9983 = ORIENTED_EDGE ( 'NONE', *, *, #11255, .T. ) ;
#9984 = AXIS2_PLACEMENT_3D ( 'NONE', #12157, #1643, #8394 ) ;
#9985 = ORIENTED_EDGE ( 'NONE', *, *, #12144, .T. ) ;
#9986 = EDGE_CURVE ( 'NONE', #4412, #6955, #1688, .T. ) ;
#9987 = DIRECTION ( 'NONE',  ( 1.000000000000000000, 0.000000000000000000, 0.000000000000000000 ) ) ;
#9988 = DIRECTION ( 'NONE',  ( 0.000000000000000000, 0.000000000000000000, 1.000000000000000000 ) ) ;
#9989 = CARTESIAN_POINT ( 'NONE',  ( 2.765633920072239516, 16.37294372382858398, 18.55949924794898465 ) ) ;
#9990 = CARTESIAN_POINT ( 'NONE',  ( 0.7592463941534229876, -3.797885586973023475, -27.31305418910213234 ) ) ;
#9991 = DIRECTION ( 'NONE',  ( -5.339417856040274462E-17, -1.063174570779084693E-17, 1.000000000000000000 ) ) ;
#9992 = CIRCLE ( 'NONE', #7034, 3.000000000000002665 ) ;
#9993 = CARTESIAN_POINT ( 'NONE',  ( 2.010451923687323283, 11.98750039041494198, 12.70439593876664652 ) ) ;
#9994 = ADVANCED_FACE ( 'NONE', ( #8182 ), #1198, .F. ) ;
#9995 = ORIENTED_EDGE ( 'NONE', *, *, #13946, .F. ) ;
#9996 = CARTESIAN_POINT ( 'NONE',  ( 0.006974771092478813939, -22.53337530003410905, 9.686319561460866367 ) ) ;
#9997 =( GEOMETRIC_REPRESENTATION_CONTEXT ( 3 ) GLOBAL_UNCERTAINTY_ASSIGNED_CONTEXT ( ( #12763 ) ) GLOBAL_UNIT_ASSIGNED_CONTEXT ( ( #13444, #1763, #6448 ) ) REPRESENTATION_CONTEXT ( 'NONE', 'WORKASPACE' ) );
#9998 = CARTESIAN_POINT ( 'NONE',  ( 2.789999999999999147, 15.47981323787947794, 0.000000000000000000 ) ) ;
#9999 = PRESENTATION_LAYER_ASSIGNMENT (  '', '', ( #1170 ) ) ;
#10000 = EDGE_LOOP ( 'NONE', ( #12530, #421, #11543, #7359 ) ) ;
#10001 = ORIENTED_EDGE ( 'NONE', *, *, #13541, .F. ) ;
#10002 = ORIENTED_EDGE ( 'NONE', *, *, #5263, .F. ) ;
#10003 = VERTEX_POINT ( 'NONE', #15117 ) ;
#10004 = CARTESIAN_POINT ( 'NONE',  ( 0.02436607992775761261, 22.71065055754452544, 9.836394144775786330 ) ) ;
#10005 = CARTESIAN_POINT ( 'NONE',  ( 2.782672467460656218, -14.24942254254687946, -2.217238903388711435 ) ) ;
#10006 = CIRCLE ( 'NONE', #14924, 5.575000000000000178 ) ;
#10007 = B_SPLINE_CURVE_WITH_KNOTS ( 'NONE', 3,
 ( #12042, #5229, #1606, #3830 ),
 .UNSPECIFIED., .F., .F.,
 ( 4, 4 ),
 ( 0.003263275852154340524, 0.003756984793530001795 ),
 .UNSPECIFIED. ) ;
#10008 = VECTOR ( 'NONE', #5218, 1000.000000000000000 ) ;
#10009 = CIRCLE ( 'NONE', #12945, 2.524999999999995914 ) ;
#10010 = LINE ( 'NONE', #7702, #1202 ) ;
#10011 = CARTESIAN_POINT ( 'NONE',  ( 18.21994936526786901, -20.29667510578869027, 4.000000000000000000 ) ) ;
#10012 = B_SPLINE_CURVE_WITH_KNOTS ( 'NONE', 3,
 ( #9348, #973, #3357, #5674, #4820, #8341 ),
 .UNSPECIFIED., .F., .F.,
 ( 4, 2, 4 ),
 ( 2.132675795043207789E-07, 0.001878604073277004988, 0.003756994878974505639 ),
 .UNSPECIFIED. ) ;
#10013 = EDGE_CURVE ( 'NONE', #5631, #4617, #6829, .T. ) ;
#10014 = ORIENTED_EDGE ( 'NONE', *, *, #1986, .T. ) ;
#10015 = CARTESIAN_POINT ( 'NONE',  ( 0.7592463941534238758, 27.31305418910209681, -3.797885586973310801 ) ) ;
#10016 = CYLINDRICAL_SURFACE ( 'NONE', #6816, 28.06981291497571362 ) ;
#10017 = CARTESIAN_POINT ( 'NONE',  ( 0.3603712044621530941, 15.53862542373106415, 5.230001598524659734 ) ) ;
#10018 = EDGE_CURVE ( 'NONE', #910, #1849, #12858, .T. ) ;
#10019=STYLED_ITEM('',(#15272),#14111);
#10020 = DIRECTION ( 'NONE',  ( -0.4036950204470267645, 0.9148936170212768060, 0.000000000000000000 ) ) ;
#10021 = CIRCLE ( 'NONE', #2172, 10.00000000000000000 ) ;
#10022 = CIRCLE ( 'NONE', #4877, 2.524999999999998135 ) ;
#10023 = ORIENTED_EDGE ( 'NONE', *, *, #5595, .F. ) ;
#10024 = DIRECTION ( 'NONE',  ( 1.000000000000000000, 0.000000000000000000, 0.000000000000000000 ) ) ;
#10025 = LINE ( 'NONE', #9865, #1339 ) ;
#10026 = ORIENTED_EDGE ( 'NONE', *, *, #4051, .F. ) ;
#10027 = ORIENTED_EDGE ( 'NONE', *, *, #2913, .F. ) ;
#10028 = DIRECTION ( 'NONE',  ( -1.000000000000000000, 0.000000000000000000, -0.000000000000000000 ) ) ;
#10029 = EDGE_CURVE ( 'NONE', #85, #11822, #10723, .T. ) ;
#10030 = EDGE_CURVE ( 'NONE', #672, #4130, #7332, .T. ) ;
#10031 = DIRECTION ( 'NONE',  ( 1.000000000000000000, 0.000000000000000000, 0.000000000000000000 ) ) ;
#10032 = CARTESIAN_POINT ( 'NONE',  ( 5.999999999999999112, 7.347880794884118750E-16, 3.000000000000000000 ) ) ;
#10033 = CIRCLE ( 'NONE', #11984, 5.899999999999999467 ) ;
#10034 = AXIS2_PLACEMENT_3D ( 'NONE', #9283, #7045, #10582 ) ;
#10035 = ORIENTED_EDGE ( 'NONE', *, *, #2192, .T. ) ;
#10036 = FACE_OUTER_BOUND ( 'NONE', #12703, .T. ) ;
#10037 = CARTESIAN_POINT ( 'NONE',  ( -14.40394475573011945, -10.79473832354794283, -3.000000000000000000 ) ) ;
#10038 = ORIENTED_EDGE ( 'NONE', *, *, #4570, .T. ) ;
#10039 =( NAMED_UNIT ( * ) SI_UNIT ( $, .STERADIAN. ) SOLID_ANGLE_UNIT ( ) );
#10040 = ORIENTED_EDGE ( 'NONE', *, *, #3701, .T. ) ;
#10041 = ORIENTED_EDGE ( 'NONE', *, *, #5323, .T. ) ;
#10042 = EDGE_CURVE ( 'NONE', #5604, #11593, #7032, .T. ) ;
#10043 = ORIENTED_EDGE ( 'NONE', *, *, #15201, .T. ) ;
#10044 = SHAPE_REPRESENTATION ( 'connector', ( #1376 ), #9175 ) ;
#10045 = B_SPLINE_CURVE_WITH_KNOTS ( 'NONE', 3,
 ( #13980, #6684, #6615, #989, #835, #3447 ),
 .UNSPECIFIED., .F., .F.,
 ( 4, 2, 4 ),
 ( 1.979325885420663486E-07, 0.001878588715165609938, 0.003756979497742677504 ),
 .UNSPECIFIED. ) ;
#10046 = CARTESIAN_POINT ( 'NONE',  ( 65.21556745095632834, 33.50594455047664866, -2.000000000000000000 ) ) ;
#10047 = AXIS2_PLACEMENT_3D ( 'NONE', #4594, #1047, #3279 ) ;
#10048 = DIRECTION ( 'NONE',  ( 1.000000000000000000, 0.000000000000000000, 0.000000000000000000 ) ) ;
#10049 = EDGE_CURVE ( 'NONE', #3458, #1390, #7176, .T. ) ;
#10050 = DIRECTION ( 'NONE',  ( 0.9148936170212769170, 0.4036950204470262649, -0.000000000000000000 ) ) ;
#10051 = CYLINDRICAL_SURFACE ( 'NONE', #7732, 8.399999999999998579 ) ;
#10052 = SHAPE_DEFINITION_REPRESENTATION ( #13372, #12685 ) ;
#10053 = DIRECTION ( 'NONE',  ( 0.000000000000000000, 0.000000000000000000, 1.000000000000000000 ) ) ;
#10054 = DIRECTION ( 'NONE',  ( 0.000000000000000000, 0.000000000000000000, -1.000000000000000000 ) ) ;
#10055 = CARTESIAN_POINT ( 'NONE',  ( 0.000000000000000000, 23.48180575137739368, -5.535312321042471062 ) ) ;
#10056 = EDGE_CURVE ( 'NONE', #3010, #6024, #6442, .T. ) ;
#10057 = VERTEX_POINT ( 'NONE', #4738 ) ;
#10058 = DIRECTION ( 'NONE',  ( -1.000000000000000000, -0.000000000000000000, 0.000000000000000000 ) ) ;
#10059 = LINE ( 'NONE', #9203, #7161 ) ;
#10060 = DIRECTION ( 'NONE',  ( -1.000000000000000000, -0.000000000000000000, -0.000000000000000000 ) ) ;
#10061 = EDGE_LOOP ( 'NONE', ( #13783, #4134, #7655, #14097 ) ) ;
#10062 = CARTESIAN_POINT ( 'NONE',  ( 2.789999999999999147, -7.739906618939614624, -13.40591150984234581 ) ) ;
#10063 = CARTESIAN_POINT ( 'NONE',  ( 2.031033465052724196, 4.828387785248403397, -27.14933624560903525 ) ) ;
#10064 = ORIENTED_EDGE ( 'NONE', *, *, #4223, .F. ) ;
#10065 = ORIENTED_EDGE ( 'NONE', *, *, #9376, .F. ) ;
#10066 = DIRECTION ( 'NONE',  ( -1.000000000000000000, -0.000000000000000000, -0.000000000000000000 ) ) ;
#10067 = CARTESIAN_POINT ( 'NONE',  ( 98.48580539929344013, 0.9022481406819604643, -2.000000000000000888 ) ) ;
#10068 = CARTESIAN_POINT ( 'NONE',  ( 1.774186184918758212E-16, 2.133490293297354956, -24.22479935914658000 ) ) ;
#10069 = CARTESIAN_POINT ( 'NONE',  ( -19.40394475573011590, -4.794738323547945491, 22.00000000000000000 ) ) ;
#10070 = AXIS2_PLACEMENT_3D ( 'NONE', #4743, #2209, #98 ) ;
#10071 = CARTESIAN_POINT ( 'NONE',  ( 2.790000000000077307, -5.456611084821691549, -23.69897269326682832 ) ) ;
#10072 = CARTESIAN_POINT ( 'NONE',  ( -20.63749999999999574, 6.613092715395707467E-16, 5.400000000000000355 ) ) ;
#10073 = CARTESIAN_POINT ( 'NONE',  ( 0.02436607992776325046, -18.55949924794904504, 16.37294372382852004 ) ) ;
#10074 = ORIENTED_EDGE ( 'NONE', *, *, #13596, .F. ) ;
#10075 = PLANE ( 'NONE',  #14396 ) ;
#10076 = LINE ( 'NONE', #14772, #10657 ) ;
#10077 = ORIENTED_EDGE ( 'NONE', *, *, #13691, .F. ) ;
#10078 =( LENGTH_UNIT ( ) NAMED_UNIT ( * ) SI_UNIT ( .MILLI., .METRE. ) );
#10079 = ORIENTED_EDGE ( 'NONE', *, *, #8434, .T. ) ;
#10080 = VERTEX_POINT ( 'NONE', #1264 ) ;
#10081 = VERTEX_POINT ( 'NONE', #5957 ) ;
#10082 = CARTESIAN_POINT ( 'NONE',  ( -17.28189153115278032, -8.313322929496736791, -3.715604213194723273E-15 ) ) ;
#10083 = DIRECTION ( 'NONE',  ( 0.000000000000000000, 0.000000000000000000, -1.000000000000000000 ) ) ;
#10084 = EDGE_CURVE ( 'NONE', #988, #14023, #10639, .T. ) ;
#10085 = CARTESIAN_POINT ( 'NONE',  ( -4.000000000000000000, 0.000000000000000000, 5.500000000000000000 ) ) ;
#10086 = DIRECTION ( 'NONE',  ( -1.000000000000000000, -0.000000000000000000, -0.000000000000000000 ) ) ;
#10087 = VERTEX_POINT ( 'NONE', #12018 ) ;
#10088 = DIRECTION ( 'NONE',  ( 0.000000000000000000, 0.000000000000000000, -1.000000000000000000 ) ) ;
#10089 = DIRECTION ( 'NONE',  ( -0.000000000000000000, -0.000000000000000000, 1.000000000000000000 ) ) ;
#10090 = CARTESIAN_POINT ( 'NONE',  ( 0.5279272304333944010, -11.57956866523235462, 24.43806413951671530 ) ) ;
#10091 = CARTESIAN_POINT ( 'NONE',  ( 0.8291131470075020493, -24.44424927289185590, 12.96989951879399072 ) ) ;
#10092 = ADVANCED_FACE ( 'NONE', ( #12254 ), #6115, .F. ) ;
#10093 = ORIENTED_EDGE ( 'NONE', *, *, #14484, .T. ) ;
#10094 = CARTESIAN_POINT ( 'NONE',  ( 86.17559721729969624, 12.01344854909570259, 7.000000000000000000 ) ) ;
#10095 = EDGE_CURVE ( 'NONE', #635, #5463, #9784, .T. ) ;
#10096 = DIRECTION ( 'NONE',  ( -1.000000000000000000, 0.000000000000000000, 0.000000000000000000 ) ) ;
#10097 = VERTEX_POINT ( 'NONE', #14501 ) ;
#10098 = ORIENTED_EDGE ( 'NONE', *, *, #13764, .T. ) ;
#10099 = CYLINDRICAL_SURFACE ( 'NONE', #15192, 8.400000000000000355 ) ;
#10100 = EDGE_CURVE ( 'NONE', #949, #14075, #4082, .T. ) ;
#10101 =( NAMED_UNIT ( * ) SI_UNIT ( $, .STERADIAN. ) SOLID_ANGLE_UNIT ( ) );
#10102 = FACE_OUTER_BOUND ( 'NONE', #8091, .T. ) ;
#10103 = EDGE_LOOP ( 'NONE', ( #14990, #10844, #358, #834, #14183, #6300, #12661, #1497 ) ) ;
#10104 = CARTESIAN_POINT ( 'NONE',  ( 2.764680872513207266, -9.232963481057685939, -11.36963888406697087 ) ) ;
#10105 = ORIENTED_EDGE ( 'NONE', *, *, #2970, .F. ) ;
#10106 = DIRECTION ( 'NONE',  ( -1.000000000000000000, -0.000000000000000000, -0.000000000000000000 ) ) ;
#10107 = CARTESIAN_POINT ( 'NONE',  ( 0.006974693931643255289, 16.17543236987988919, 18.43727551351037519 ) ) ;
#10108 = ORIENTED_EDGE ( 'NONE', *, *, #8414, .F. ) ;
#10109 = CARTESIAN_POINT ( 'NONE',  ( 2.789999999999999147, 24.34211360614310848, -7.909232158574561744 ) ) ;
#10110 = EDGE_CURVE ( 'NONE', #3838, #4613, #1425, .T. ) ;
#10111 = ORIENTED_EDGE ( 'NONE', *, *, #14144, .T. ) ;
#10112 = ORIENTED_EDGE ( 'NONE', *, *, #2644, .T. ) ;
#10113 = VECTOR ( 'NONE', #12350, 1000.000000000000000 ) ;
#10114 = EDGE_LOOP ( 'NONE', ( #13994, #9486, #4539, #14970 ) ) ;
#10115 = CARTESIAN_POINT ( 'NONE',  ( 2.031033471609898111, 3.797536611356316705, 27.31260702007176988 ) ) ;
#10116 = LINE ( 'NONE', #1043, #5123 ) ;
#10117 = ADVANCED_FACE ( 'NONE', ( #9869 ), #3798, .T. ) ;
#10118 = DIRECTION ( 'NONE',  ( -0.000000000000000000, -0.000000000000000000, 1.000000000000000000 ) ) ;
#10119 = CARTESIAN_POINT ( 'NONE',  ( 2.764680872513207266, -9.232963481057685939, -11.36963888406697087 ) ) ;
#10120 = APPLICATION_PROTOCOL_DEFINITION ( 'draft international standard', 'automotive_design', 1998, #2034 ) ;
#10121 = DIRECTION ( 'NONE',  ( 0.000000000000000000, 0.000000000000000000, 1.000000000000000000 ) ) ;
#10122 = CARTESIAN_POINT ( 'NONE',  ( 0.1855657168891852171, 22.53097606933003405, -12.84444904262000975 ) ) ;
#10123 = DIRECTION ( 'NONE',  ( -0.000000000000000000, -0.000000000000000000, -1.000000000000000000 ) ) ;
#10124 = ADVANCED_FACE ( 'NONE', ( #6184 ), #3962, .F. ) ;
#10125 = ORIENTED_EDGE ( 'NONE', *, *, #6440, .F. ) ;
#10127 = VECTOR ( 'NONE', #9218, 1000.000000000000000 ) ;
#10126 = CARTESIAN_POINT ( 'NONE',  ( 2.789999999999999147, 5.229914364928542447, -13.68080036884343009 ) ) ;
#10128 = TOROIDAL_SURFACE ( 'NONE', #3291, 14.01039946648074341, 8.000000000000000000 ) ;
#10129 = DIRECTION ( 'NONE',  ( -1.000000000000000000, -0.000000000000000000, -0.000000000000000000 ) ) ;
#10130 = FACE_OUTER_BOUND ( 'NONE', #153, .T. ) ;
#10131 = ADVANCED_FACE ( 'NONE', ( #4033, #11097, #13172, #9946, #1653, #3884, #1499 ), #8708, .F. ) ;
#10132 = EDGE_CURVE ( 'NONE', #4420, #6654, #6340, .T. ) ;
#10133 = VERTEX_POINT ( 'NONE', #5130 ) ;
#10134 = CARTESIAN_POINT ( 'NONE',  ( 13.28797974610714761, -21.11867004231547540, 3.000000000000002665 ) ) ;
#10135 = CARTESIAN_POINT ( 'NONE',  ( 2.783025336474040934, -21.08118142846912235, 12.53640742967745858 ) ) ;
#10136 = ORIENTED_EDGE ( 'NONE', *, *, #10132, .T. ) ;
#10137 = ORIENTED_EDGE ( 'NONE', *, *, #4204, .F. ) ;
#10138 = FACE_OUTER_BOUND ( 'NONE', #4721, .T. ) ;
#10139 = CARTESIAN_POINT ( 'NONE',  ( -16.80212006966224791, -13.74240776967763900, -3.794707603699265519E-15 ) ) ;
#10140 = AXIS2_PLACEMENT_3D ( 'NONE', #11560, #10406, #3710 ) ;
#10141 = CARTESIAN_POINT ( 'NONE',  ( 2.782672467460654442, 2.217238903388760285, -14.24942254254687057 ) ) ;
#10142 = CARTESIAN_POINT ( 'NONE',  ( 0.1882238946918232125, -2.857713464478510268, -25.78859396478530996 ) ) ;
#10143 = CYLINDRICAL_SURFACE ( 'NONE', #12383, 28.06981291497571362 ) ;
#10144 = CARTESIAN_POINT ( 'NONE',  ( 1.039999999999996705, -19.67366047555515252, -20.02152543075367319 ) ) ;
#10145 = CARTESIAN_POINT ( 'NONE',  ( 2.765633920072238627, 5.391175441198956086, -24.15498966839956907 ) ) ;
#10146 = EDGE_CURVE ( 'NONE', #11722, #14952, #4985, .T. ) ;
#10147 = VERTEX_POINT ( 'NONE', #13401 ) ;
#10148 = CARTESIAN_POINT ( 'NONE',  ( -18.40394475573011945, -10.79473832354794460, 0.7999999999999961586 ) ) ;
#10149 = LINE ( 'NONE', #6693, #5283 ) ;
#10150 = EDGE_CURVE ( 'NONE', #1390, #1547, #13210, .T. ) ;
#10151 = ORIENTED_EDGE ( 'NONE', *, *, #13139, .T. ) ;
#10152 =( NAMED_UNIT ( * ) SI_UNIT ( $, .STERADIAN. ) SOLID_ANGLE_UNIT ( ) );
#10153 = ORIENTED_EDGE ( 'NONE', *, *, #14469, .F. ) ;
#10154 = ORIENTED_EDGE ( 'NONE', *, *, #5346, .F. ) ;
#10155 = VERTEX_POINT ( 'NONE', #1568 ) ;
#10156 = DIRECTION ( 'NONE',  ( 1.000000000000000000, -0.000000000000000000, -0.000000000000000000 ) ) ;
#10157 = DIRECTION ( 'NONE',  ( 0.000000000000000000, 0.000000000000000000, -1.000000000000000000 ) ) ;
#10158 = ADVANCED_FACE ( 'NONE', ( #5205 ), #10941, .T. ) ;
#10159 = CYLINDRICAL_SURFACE ( 'NONE', #12257, 17.95481323787947403 ) ;
#10160 = ORIENTED_EDGE ( 'NONE', *, *, #10286, .F. ) ;
#10161 = CYLINDRICAL_SURFACE ( 'NONE', #15100, 2.999999999999975131 ) ;
#10162 = DIRECTION ( 'NONE',  ( -1.000000000000000000, 0.000000000000000000, -0.000000000000000000 ) ) ;
#10163 = EDGE_CURVE ( 'NONE', #7854, #13647, #2395, .T. ) ;
#10164 = LINE ( 'NONE', #7789, #14337 ) ;
#10165 = LINE ( 'NONE', #6641, #291 ) ;
#10166 = ADVANCED_FACE ( 'NONE', ( #14332 ), #487, .F. ) ;
#10167 = VECTOR ( 'NONE', #7618, 1000.000000000000000 ) ;
#10168 = AXIS2_PLACEMENT_3D ( 'NONE', #14617, #14322, #12371 ) ;
#10169 = ORIENTED_EDGE ( 'NONE', *, *, #4453, .T. ) ;
#10170 = DIRECTION ( 'NONE',  ( -1.000000000000000000, -0.000000000000000000, -0.000000000000000000 ) ) ;
#10171 = CARTESIAN_POINT ( 'NONE',  ( 1.749999999999999778, -17.29145405592692342, 4.835383649608411716 ) ) ;
#10172 = ORIENTED_EDGE ( 'NONE', *, *, #80, .F. ) ;
#10173 = ORIENTED_EDGE ( 'NONE', *, *, #1384, .T. ) ;
#10174 = B_SPLINE_CURVE_WITH_KNOTS ( 'NONE', 3,
 ( #2306, #9603, #3686, #1380 ),
 .UNSPECIFIED., .F., .F.,
 ( 4, 4 ),
 ( 2.135345996173297489E-07, 0.0006888010880210770339 ),
 .UNSPECIFIED. ) ;
#10175 = CARTESIAN_POINT ( 'NONE',  ( 0.02531912748606271468, -5.229914364928256454, -13.68080036884353845 ) ) ;
#10176 = AXIS2_PLACEMENT_3D ( 'NONE', #2018, #1951, #7934 ) ;
#10177 = ORIENTED_EDGE ( 'NONE', *, *, #2929, .F. ) ;
#10178 = VECTOR ( 'NONE', #7986, 1000.000000000000114 ) ;
#10179 = DIRECTION ( 'NONE',  ( -0.000000000000000000, -1.000000000000000000, -0.000000000000000000 ) ) ;
#10180 = TOROIDAL_SURFACE ( 'NONE', #11149, 14.01039946648073986, 8.000000000000000000 ) ;
#10181 = EDGE_CURVE ( 'NONE', #7983, #14141, #2658, .T. ) ;
#10182 = EDGE_LOOP ( 'NONE', ( #14349, #2981, #4424, #2532 ) ) ;
#10183 = DIRECTION ( 'NONE',  ( 0.000000000000000000, 0.000000000000000000, 1.000000000000000000 ) ) ;
#10184 = DIRECTION ( 'NONE',  ( 0.000000000000000000, 0.000000000000000000, 1.000000000000000000 ) ) ;
#10185 = ORIENTED_EDGE ( 'NONE', *, *, #1782, .T. ) ;
#10186 = DIRECTION ( 'NONE',  ( 1.000000000000000000, 0.000000000000000000, 0.000000000000000000 ) ) ;
#10187 = VERTEX_POINT ( 'NONE', #4264 ) ;
#10188 = AXIS2_PLACEMENT_3D ( 'NONE', #116, #9515, #5153 ) ;
#10189 = ORIENTED_EDGE ( 'NONE', *, *, #2913, .T. ) ;
#10190 = AXIS2_PLACEMENT_3D ( 'NONE', #7243, #10779, #11770 ) ;
#10191 = VERTEX_POINT ( 'NONE', #14000 ) ;
#10192 = CYLINDRICAL_SURFACE ( 'NONE', #8041, 13.19999999999999929 ) ;
#10193 = CYLINDRICAL_SURFACE ( 'NONE', #12944, 28.06981291497571362 ) ;
#10194 = B_SPLINE_CURVE_WITH_KNOTS ( 'NONE', 3,
 ( #13982, #12882, #2294, #5844 ),
 .UNSPECIFIED., .F., .F.,
 ( 4, 4 ),
 ( 1.981826382900847290E-07, 0.0006887856082032348722 ),
 .UNSPECIFIED. ) ;
#10195 = FACE_OUTER_BOUND ( 'NONE', #7263, .T. ) ;
#10196 = DIRECTION ( 'NONE',  ( 0.000000000000000000, 0.000000000000000000, -1.000000000000000000 ) ) ;
#10197 = ITEM_DEFINED_TRANSFORMATION ( 'NONE', 'NONE', #10640,  #1376 ) ;
#10198 = FACE_OUTER_BOUND ( 'NONE', #12049, .T. ) ;
#10199 = LINE ( 'NONE', #14896, #4428 ) ;
#10200 = AXIS2_PLACEMENT_3D ( 'NONE', #8482, #9722, #8712 ) ;
#10201 = ORIENTED_EDGE ( 'NONE', *, *, #1121, .T. ) ;
#10202 = CARTESIAN_POINT ( 'NONE',  ( 8.000000000000000000, 0.000000000000000000, 0.000000000000000000 ) ) ;
#10203 = CARTESIAN_POINT ( 'NONE',  ( 0.02436607992776368414, -9.836394144775550075, -22.71065055754462492 ) ) ;
#10204 = CARTESIAN_POINT ( 'NONE',  ( 2.782650494170369804, -5.204557061642381299, 13.44926448535264463 ) ) ;
#10205 = ORIENTED_EDGE ( 'NONE', *, *, #10975, .F. ) ;
#10206 = EDGE_CURVE ( 'NONE', #9372, #7839, #10274, .T. ) ;
#10207 = FACE_OUTER_BOUND ( 'NONE', #14846, .T. ) ;
#10208 = CARTESIAN_POINT ( 'NONE',  ( 0.006974693931642682830, -16.17543236987975064, -18.43727551351049598 ) ) ;
#10209 = ORIENTED_EDGE ( 'NONE', *, *, #742, .F. ) ;
#10210 = ORIENTED_EDGE ( 'NONE', *, *, #4957, .F. ) ;
#10211 = DIRECTION ( 'NONE',  ( 0.000000000000000000, 0.000000000000000000, 1.000000000000000000 ) ) ;
#10212 = CARTESIAN_POINT ( 'NONE',  ( 2.781248467067199748, -13.40591150984217705, -5.214906618939849636 ) ) ;
#10213 = ORIENTED_EDGE ( 'NONE', *, *, #7007, .F. ) ;
#10214 = CARTESIAN_POINT ( 'NONE',  ( 2.010451919658892361, -16.99607982911243909, 4.029281904976570239 ) ) ;
#10215 = DIRECTION ( 'NONE',  ( 1.000000000000000000, -0.000000000000000000, -0.000000000000000000 ) ) ;
#10216 = CARTESIAN_POINT ( 'NONE',  ( 2.783025342027735327, -5.408388659523925668, -23.92335783895643075 ) ) ;
#10217 = ADVANCED_FACE ( 'NONE', ( #8153 ), #4642, .T. ) ;
#10218 = EDGE_CURVE ( 'NONE', #1632, #7996, #10022, .T. ) ;
#10219 = CARTESIAN_POINT ( 'NONE',  ( 4.872650870659752442, 0.4273491293402468805, 0.000000000000000000 ) ) ;
#10220 = CARTESIAN_POINT ( 'NONE',  ( 0.02436607992776151574, 24.15498966839970052, -5.391175441198366336 ) ) ;
#10221 = VERTEX_POINT ( 'NONE', #11605 ) ;
#10222 = AXIS2_PLACEMENT_3D ( 'NONE', #10533, #8193, #4701 ) ;
#10223 = DIRECTION ( 'NONE',  ( 0.000000000000000000, 0.000000000000000000, 1.000000000000000000 ) ) ;
#10224 = AXIS2_PLACEMENT_3D ( 'NONE', #981, #2060, #679 ) ;
#10225 = CARTESIAN_POINT ( 'NONE',  ( 0.02436607992776108206, -24.15498966839966855, 5.391175441198523544 ) ) ;
#10226 = B_SPLINE_CURVE_WITH_KNOTS ( 'NONE', 3,
 ( #9354, #4826, #10734, #192 ),
 .UNSPECIFIED., .F., .F.,
 ( 4, 4 ),
 ( 3.059063720746937335E-07, 0.0006888942284914101538 ),
 .UNSPECIFIED. ) ;
#10227 = ORIENTED_EDGE ( 'NONE', *, *, #6171, .F. ) ;
#10228 = ORIENTED_EDGE ( 'NONE', *, *, #3382, .T. ) ;
#10229 = ORIENTED_EDGE ( 'NONE', *, *, #7737, .T. ) ;
#10230 = EDGE_LOOP ( 'NONE', ( #5203, #2305, #1938, #11764, #5128, #6214, #10249, #13458 ) ) ;
#10231 = ADVANCED_FACE ( 'NONE', ( #4194 ), #10099, .T. ) ;
#10232 = CARTESIAN_POINT ( 'NONE',  ( 2.010451923687323283, -12.70439593876669271, 11.98750039041489224 ) ) ;
#10233 = EDGE_CURVE ( 'NONE', #6410, #14061, #11971, .T. ) ;
#10234 = CARTESIAN_POINT ( 'NONE',  ( 1.150000000000000577, 0.000000000000000000, 0.000000000000000000 ) ) ;
#10235 = AXIS2_PLACEMENT_3D ( 'NONE', #9058, #6745, #11424 ) ;
#10236 = VECTOR ( 'NONE', #1243, 1000.000000000000000 ) ;
#10237 = CARTESIAN_POINT ( 'NONE',  ( 1.749999999999998002, -27.68468304288255766, -4.633866840649213614 ) ) ;
#10238 = EDGE_CURVE ( 'NONE', #2494, #8331, #3890, .T. ) ;
#10239 = AXIS2_PLACEMENT_3D ( 'NONE', #12522, #10066, #13895 ) ;
#10240 = CARTESIAN_POINT ( 'NONE',  ( -1.000000000000000222, -4.808326913195983821, 0.000000000000000000 ) ) ;
#10241 = AXIS2_PLACEMENT_3D ( 'NONE', #3213, #968, #5669 ) ;
#10242 = ORIENTED_EDGE ( 'NONE', *, *, #1070, .T. ) ;
#10243 = CARTESIAN_POINT ( 'NONE',  ( 14.40394475573011945, -10.79473832354794460, 6.000000000000000000 ) ) ;
#10244 = DIRECTION ( 'NONE',  ( 0.000000000000000000, 0.000000000000000000, 1.000000000000000000 ) ) ;
#10245 = EDGE_CURVE ( 'NONE', #5872, #8109, #12486, .T. ) ;
#10246 = AXIS2_PLACEMENT_3D ( 'NONE', #14251, #13003, #5950 ) ;
#10247 = CARTESIAN_POINT ( 'NONE',  ( 2.764680872515352661, -2.311161484776655950, 14.46287784598616355 ) ) ;
#10248 = AXIS2_PLACEMENT_3D ( 'NONE', #1356, #13104, #2591 ) ;
#10249 = ORIENTED_EDGE ( 'NONE', *, *, #249, .T. ) ;
#10250 = MECHANICAL_DESIGN_GEOMETRIC_PRESENTATION_REPRESENTATION (  '', ( #1915 ), #3873 ) ;
#10251 = CARTESIAN_POINT ( 'NONE',  ( 0.000000000000000000, -7.739906618939802918, 13.40591150984224100 ) ) ;
#10252 = CARTESIAN_POINT ( 'NONE',  ( 2.789999999999999147, 11.04103753892283635, -8.624777288397684316 ) ) ;
#10253 = AXIS2_PLACEMENT_3D ( 'NONE', #6506, #664, #2678 ) ;
#10254 = VERTEX_POINT ( 'NONE', #14794 ) ;
#10255 = EDGE_LOOP ( 'NONE', ( #11562, #9436, #18, #9212 ) ) ;
#10256 = VECTOR ( 'NONE', #14573, 1000.000000000000000 ) ;
#10257 =( LENGTH_UNIT ( ) NAMED_UNIT ( * ) SI_UNIT ( .MILLI., .METRE. ) );
#10258 = CARTESIAN_POINT ( 'NONE',  ( 0.000000000000000000, 0.000000000000000000, 4.500000000000000888 ) ) ;
#10259 = EDGE_LOOP ( 'NONE', ( #14512, #11772, #12228, #12444, #1205, #13419, #2005 ) ) ;
#10260 = DIRECTION ( 'NONE',  ( -1.000000000000000000, 0.000000000000000000, 0.000000000000000000 ) ) ;
#10261 = DIRECTION ( 'NONE',  ( 0.000000000000000000, 0.000000000000000000, 1.000000000000000000 ) ) ;
#10262 = DIRECTION ( 'NONE',  ( 0.000000000000000000, -0.3090169943749406234, -0.9510565162951558627 ) ) ;
#10263 = CIRCLE ( 'NONE', #4377, 14.01039946648074341 ) ;
#10264 = AXIS2_PLACEMENT_3D ( 'NONE', #14215, #13846, #6863 ) ;
#10265 = ORIENTED_EDGE ( 'NONE', *, *, #14631, .F. ) ;
#10266 = B_SPLINE_CURVE_WITH_KNOTS ( 'NONE', 3,
 ( #7226, #9605, #3531, #4860 ),
 .UNSPECIFIED., .F., .F.,
 ( 4, 4 ),
 ( 0.005123713096549374624, 0.005814346476695759873 ),
 .UNSPECIFIED. ) ;
#10267 = CARTESIAN_POINT ( 'NONE',  ( 1.749999999999998002, 12.96210679857786552, 24.89775460606837143 ) ) ;
#10268 = VERTEX_POINT ( 'NONE', #12322 ) ;
#10269 = ORIENTED_EDGE ( 'NONE', *, *, #4217, .F. ) ;
#10270 = ORIENTED_EDGE ( 'NONE', *, *, #7835, .T. ) ;
#10271 = SURFACE_SIDE_STYLE ('',( #885 ) ) ;
#10272 = LINE ( 'NONE', #13573, #12224 ) ;
#10273 = CARTESIAN_POINT ( 'NONE',  ( 61.98919079003883326, 3.953582723775848962, 2.999999999999999112 ) ) ;
#10274 = CIRCLE ( 'NONE', #2418, 28.06981291497571362 ) ;
#10275 = CARTESIAN_POINT ( 'NONE',  ( -14.40394475573011945, -10.79473832354794460, 0.7999999999999960476 ) ) ;
#10276 = CIRCLE ( 'NONE', #3641, 3.799999999999999378 ) ;
#10277 = DIRECTION ( 'NONE',  ( -1.000000000000000000, 0.000000000000000000, 0.000000000000000000 ) ) ;
#10278 = DIRECTION ( 'NONE',  ( -1.000000000000000000, -0.000000000000000000, -0.000000000000000000 ) ) ;
#10279 = VERTEX_POINT ( 'NONE', #5863 ) ;
#10280 = CARTESIAN_POINT ( 'NONE',  ( 14.27437366993929579, -27.03703358530833967, -2.000000000000000000 ) ) ;
#10281 = B_SPLINE_CURVE_WITH_KNOTS ( 'NONE', 3,
 ( #13202, #1680, #11049, #432, #6364, #5075 ),
 .UNSPECIFIED., .F., .F.,
 ( 4, 2, 4 ),
 ( 2.032124546189621919E-07, 0.001878594002992312268, 0.003756984793530005265 ),
 .UNSPECIFIED. ) ;
#10282 = LINE ( 'NONE', #8894, #534 ) ;
#10283 = CARTESIAN_POINT ( 'NONE',  ( 0.02531912748286561932, 13.68080036884348516, 5.229914364928400339 ) ) ;
#10284 = EDGE_LOOP ( 'NONE', ( #3775, #1375, #513, #14770 ) ) ;
#10285 = VECTOR ( 'NONE', #10333, 1000.000000000000000 ) ;
#10286 = EDGE_CURVE ( 'NONE', #11305, #12316, #11251, .T. ) ;
#10287 = DIRECTION ( 'NONE',  ( 0.000000000000000000, 0.000000000000000000, 1.000000000000000000 ) ) ;
#10288 = CARTESIAN_POINT ( 'NONE',  ( 2.790000000000076419, -20.85287692521938752, 12.51293083811791718 ) ) ;
#10289 = EDGE_LOOP ( 'NONE', ( #5159, #8474, #13534, #10831 ) ) ;
#10290 = EDGE_LOOP ( 'NONE', ( #2684, #6808, #9600, #4949 ) ) ;
#10291 = CARTESIAN_POINT ( 'NONE',  ( 0.5431871499410856341, 5.154374911959137329, -16.16568790143436019 ) ) ;
#10292 = CARTESIAN_POINT ( 'NONE',  ( 2.789999999999999147, 24.63872515616082737, -2.336989772644355590 ) ) ;
#10293 = EDGE_CURVE ( 'NONE', #9857, #5968, #3859, .T. ) ;
#10294 = EDGE_LOOP ( 'NONE', ( #4259, #1494, #4481, #8440 ) ) ;
#10295 = CARTESIAN_POINT ( 'NONE',  ( 0.000000000000000000, -13.87420763704362869, 1.948757464274129214 ) ) ;
#10296 = LINE ( 'NONE', #2293, #4289 ) ;
#10297 = LINE ( 'NONE', #4233, #13614 ) ;
#10298 = ADVANCED_FACE ( 'NONE', ( #10546 ), #9379, .F. ) ;
#10299 = CARTESIAN_POINT ( 'NONE',  ( 0.5321745087963413168, -24.44564404695853455, 11.58891744060097295 ) ) ;
#10300 = FACE_OUTER_BOUND ( 'NONE', #12836, .T. ) ;
#10301 = VECTOR ( 'NONE', #5418, 1000.000000000000000 ) ;
#10302 = ORIENTED_EDGE ( 'NONE', *, *, #4714, .T. ) ;
#10303 = DIRECTION ( 'NONE',  ( -1.000000000000000000, -0.000000000000000000, 0.000000000000000000 ) ) ;
#10304 = CARTESIAN_POINT ( 'NONE',  ( 2.790000000000060876, -2.096282088614865646, 14.05326139264726848 ) ) ;
#10305 = ORIENTED_EDGE ( 'NONE', *, *, #4604, .T. ) ;
#10306 = EDGE_CURVE ( 'NONE', #9372, #8828, #13555, .T. ) ;
#10307 =( NAMED_UNIT ( * ) SI_UNIT ( $, .STERADIAN. ) SOLID_ANGLE_UNIT ( ) );
#10308 = EDGE_CURVE ( 'NONE', #7147, #10776, #5866, .T. ) ;
#10309 = ORIENTED_EDGE ( 'NONE', *, *, #4665, .T. ) ;
#10310 = VERTEX_POINT ( 'NONE', #2 ) ;
#10311 = ORIENTED_EDGE ( 'NONE', *, *, #8983, .T. ) ;
#10312 = VECTOR ( 'NONE', #8590, 1000.000000000000000 ) ;
#10313 = CARTESIAN_POINT ( 'NONE',  ( 20.40394475573011590, -10.79473832354794460, 3.000000000000000000 ) ) ;
#10314 = CARTESIAN_POINT ( 'NONE',  ( 0.5279272304333941790, -24.43806413951667622, -11.57956866523244166 ) ) ;
#10315 = CARTESIAN_POINT ( 'NONE',  ( 0.7686372158811271005, -11.98841295390588435, -12.71987259277447180 ) ) ;
#10316 = CARTESIAN_POINT ( 'NONE',  ( 0.02531912748631468327, -14.46287784598615644, -2.311161484776706576 ) ) ;
#10317 = ORIENTED_EDGE ( 'NONE', *, *, #14233, .T. ) ;
#10318 = CARTESIAN_POINT ( 'NONE',  ( 0.5279272304333949561, 24.43806413951675793, 11.57956866523226580 ) ) ;
#10319 = DIRECTION ( 'NONE',  ( 0.02857142857142857054, 0.9995917534020515305, 0.000000000000000000 ) ) ;
#10320 = ADVANCED_FACE ( 'NONE', ( #11323 ), #1011, .T. ) ;
#10321 = DIRECTION ( 'NONE',  ( -0.9237280213470681067, -0.3830490080632377725, 0.000000000000000000 ) ) ;
#10322 = ADVANCED_FACE ( 'NONE', ( #2244 ), #2310, .T. ) ;
#10323 = ADVANCED_FACE ( 'NONE', ( #7001 ), #13709, .T. ) ;
#10324 = ORIENTED_EDGE ( 'NONE', *, *, #14987, .F. ) ;
#10325 = CARTESIAN_POINT ( 'NONE',  ( 2.789999999999999147, 11.07980565117280314, -9.999777909379972129 ) ) ;
#10326 = PRODUCT_DEFINITION_SHAPE ( 'NONE', 'NONE',  #12070 ) ;
#10327 = CARTESIAN_POINT ( 'NONE',  ( 0.9999999999999997780, -6.008326913195983998, -0.8000000000000000444 ) ) ;
#10328 = VERTEX_POINT ( 'NONE', #14302 ) ;
#10329 = ORIENTED_EDGE ( 'NONE', *, *, #7007, .T. ) ;
#10330 = ADVANCED_FACE ( 'NONE', ( #6153 ), #9683, .F. ) ;
#10331 = CARTESIAN_POINT ( 'NONE',  ( 56.98919079003883326, 3.953582723775848962, -2.000000000000000888 ) ) ;
#10332 = ORIENTED_EDGE ( 'NONE', *, *, #3663, .T. ) ;
#10333 = DIRECTION ( 'NONE',  ( -1.000000000000000000, 0.000000000000000000, 0.000000000000000000 ) ) ;
#10334 = CARTESIAN_POINT ( 'NONE',  ( -0.1085714285714285687, -3.798448662927795372, -0.8000000000000000444 ) ) ;
#10335 = CARTESIAN_POINT ( 'NONE',  ( 10.00000000000000178, -1.390791565672601315, -131.1575142076926852 ) ) ;
#10336 = ORIENTED_EDGE ( 'NONE', *, *, #13988, .F. ) ;
#10337 = CARTESIAN_POINT ( 'NONE',  ( 31.51081190520435626, 3.030430839836910639, 6.000000000000000000 ) ) ;
#10338 = EDGE_LOOP ( 'NONE', ( #2585, #10720, #3262, #7222, #6315, #9136, #323, #2796 ) ) ;
#10339 = ORIENTED_EDGE ( 'NONE', *, *, #1979, .T. ) ;
#10340 = CARTESIAN_POINT ( 'NONE',  ( 1.749999999999998002, -24.89775460606842117, 12.96210679857777137 ) ) ;
#10341 = ADVANCED_FACE ( 'NONE', ( #8372 ), #6226, .F. ) ;
#10342 = CARTESIAN_POINT ( 'NONE',  ( 1.150000000000001688, 7.347880794884120722E-16, 6.000000000000000888 ) ) ;
#10343 = CARTESIAN_POINT ( 'NONE',  ( 0.9659243001600011924, 24.74770846292485516, 12.96726489871199028 ) ) ;
#10344 = CONTEXT_DEPENDENT_SHAPE_REPRESENTATION ( #4407, #6037 ) ;
#10345 = CARTESIAN_POINT ( 'NONE',  ( 10.00000000000000178, -1.390791565672601315, 4.000000000000003553 ) ) ;
#10346 = FACE_OUTER_BOUND ( 'NONE', #7941, .T. ) ;
#10347 = ORIENTED_EDGE ( 'NONE', *, *, #4118, .F. ) ;
#10348 = FACE_OUTER_BOUND ( 'NONE', #13126, .T. ) ;
#10349 = DIRECTION ( 'NONE',  ( -1.000000000000000000, 0.000000000000000000, -0.000000000000000000 ) ) ;
#10350 = DIRECTION ( 'NONE',  ( -0.000000000000000000, -0.000000000000000000, -1.000000000000000000 ) ) ;
#10351 = CIRCLE ( 'NONE', #5944, 6.000000000000005329 ) ;
#10352 = ORIENTED_EDGE ( 'NONE', *, *, #1686, .T. ) ;
#10353 = EDGE_CURVE ( 'NONE', #10147, #1055, #7155, .T. ) ;
#10354 = CARTESIAN_POINT ( 'NONE',  ( 88.46153288930041469, 16.46030115554384565, 6.000000000000000000 ) ) ;
#10355 = CARTESIAN_POINT ( 'NONE',  ( 2.765633920072238627, 12.59161484032942901, -21.30679549418617924 ) ) ;
#10356 = ORIENTED_EDGE ( 'NONE', *, *, #11904, .F. ) ;
#10357 = EDGE_LOOP ( 'NONE', ( #5992, #12441, #3122, #10209 ) ) ;
#10358 = CARTESIAN_POINT ( 'NONE',  ( 8.000000000000000000, 0.000000000000000000, 0.000000000000000000 ) ) ;
#10359 = DIRECTION ( 'NONE',  ( 1.000000000000000000, -0.000000000000000000, -0.000000000000000000 ) ) ;
#10360 = ORIENTED_EDGE ( 'NONE', *, *, #10432, .T. ) ;
#10361 = DIRECTION ( 'NONE',  ( -1.000000000000000000, -0.000000000000000000, 0.000000000000000000 ) ) ;
#10362 = LINE ( 'NONE', #12526, #13848 ) ;
#10363 = B_SPLINE_CURVE_WITH_KNOTS ( 'NONE', 3,
 ( #3190, #10390, #9100, #2024, #13933, #10475 ),
 .UNSPECIFIED., .F., .F.,
 ( 4, 2, 4 ),
 ( 1.979325885420528755E-07, 0.001878588715165608204, 0.003756979497742674035 ),
 .UNSPECIFIED. ) ;
#10364 = CARTESIAN_POINT ( 'NONE',  ( 2.789895104907798906, 20.67847077765723185, -12.51925356660737876 ) ) ;
#10365 = AXIS2_PLACEMENT_3D ( 'NONE', #6562, #5567, #13625 ) ;
#10366 = CIRCLE ( 'NONE', #14300, 1.999999999999998890 ) ;
#10367 = CARTESIAN_POINT ( 'NONE',  ( 0.02436607992775978102, -12.59161484032896361, -21.30679549418645280 ) ) ;
#10368 = CARTESIAN_POINT ( 'NONE',  ( 1.960886852992457241, 24.44424927289185945, 12.96989951879416125 ) ) ;
#10369 = EDGE_CURVE ( 'NONE', #4549, #1993, #1538, .T. ) ;
#10370 = ORIENTED_EDGE ( 'NONE', *, *, #7629, .F. ) ;
#10371 = DIRECTION ( 'NONE',  ( 1.000000000000000000, 1.445602896647338917E-16, -0.000000000000000000 ) ) ;
#10372 = DIRECTION ( 'NONE',  ( -1.000000000000000000, -0.000000000000000000, -0.000000000000000000 ) ) ;
#10373 = EDGE_CURVE ( 'NONE', #11075, #960, #8085, .T. ) ;
#10374 = VERTEX_POINT ( 'NONE', #7227 ) ;
#10375 = VECTOR ( 'NONE', #5977, 1000.000000000000000 ) ;
#10376 = EDGE_LOOP ( 'NONE', ( #13286, #4686, #584, #12146, #14551, #2535 ) ) ;
#10377 = ORIENTED_EDGE ( 'NONE', *, *, #12208, .F. ) ;
#10378 = EDGE_LOOP ( 'NONE', ( #10305, #13834 ) ) ;
#10379 = CARTESIAN_POINT ( 'NONE',  ( 0.007349505829628827543, -5.204557061642193005, -13.44926448535271568 ) ) ;
#10380 = CARTESIAN_POINT ( 'NONE',  ( 0.000000000000000000, 0.000000000000000000, -7.000000000000007994 ) ) ;
#10381 = CARTESIAN_POINT ( 'NONE',  ( 1.749999999999998002, 27.76164181293051669, -4.147968289691384314 ) ) ;
#10382 = DIRECTION ( 'NONE',  ( 0.000000000000000000, 0.000000000000000000, 1.000000000000000000 ) ) ;
#10383 = VECTOR ( 'NONE', #8953, 1000.000000000000114 ) ;
#10384 = DIRECTION ( 'NONE',  ( 0.000000000000000000, 0.000000000000000000, -1.000000000000000000 ) ) ;
#10385 = VERTEX_POINT ( 'NONE', #14383 ) ;
#10386 = CYLINDRICAL_SURFACE ( 'NONE', #1419, 11.66666666666667318 ) ;
#10387 = CARTESIAN_POINT ( 'NONE',  ( 1.149999999999998135, 0.000000000000000000, 0.000000000000000000 ) ) ;
#10388 = EDGE_CURVE ( 'NONE', #6042, #14329, #14310, .T. ) ;
#10389 = ORIENTED_EDGE ( 'NONE', *, *, #14425, .F. ) ;
#10390 = CARTESIAN_POINT ( 'NONE',  ( 0.07186815222488071586, -5.344160105508533931, -24.78765742476144140 ) ) ;
#10391 = DIRECTION ( 'NONE',  ( -1.000000000000000000, -0.000000000000000000, -0.000000000000000000 ) ) ;
#10392 = EDGE_LOOP ( 'NONE', ( #12226, #8803, #13938, #8368, #2026, #6048, #4262 ) ) ;
#10393 = VERTEX_POINT ( 'NONE', #5997 ) ;
#10394 = DIRECTION ( 'NONE',  ( 0.000000000000000000, 0.000000000000000000, 1.000000000000000000 ) ) ;
#10395 = EDGE_CURVE ( 'NONE', #5489, #9019, #7229, .T. ) ;
#10396 = EDGE_CURVE ( 'NONE', #13819, #7470, #13351, .T. ) ;
#10397 = ORIENTED_EDGE ( 'NONE', *, *, #3175, .F. ) ;
#10398 = CARTESIAN_POINT ( 'NONE',  ( 1.749999999999999778, -12.55714665599977842, -12.83329210556845190 ) ) ;
#10399 = CLOSED_SHELL ( 'NONE', ( #15068, #2919, #593, #9305, #11522, #2335, #857, #2562, #4766, #11540, #10131, #14054, #7517, #4131, #5931, #5723, #8677, #9570, #12807, #12707, #14286, #6416, #14347, #4496, #11597, #4699, #1474, #13735, #13325, #7565, #5907, #7412, #13861, #4982, #13969, #5442, #6144, #14017, #3048, #14260, #9525, #2980, #1956, #14199, #10330, #7179, #6190, #14758, #4451, #12833, #1179, #8714, #5969, #7411, #11512, #8948 ) ) ;
#10400 = CARTESIAN_POINT ( 'NONE',  ( 61.98919079003883326, 3.953582723775848962, 6.000000000000000000 ) ) ;
#10401 = CARTESIAN_POINT ( 'NONE',  ( -6.000000000000000888, 7.347880794884120722E-16, 4.500000000000000888 ) ) ;
#10402 = CARTESIAN_POINT ( 'NONE',  ( 2.361335444912569859, -15.76776810790841310, 5.200734291367588469 ) ) ;
#10403 = TOROIDAL_SURFACE ( 'NONE', #14610, 24.12539914357697413, 8.000000000000000000 ) ;
#10404 = CIRCLE ( 'NONE', #1576, 3.000000000000002665 ) ;
#10405 = ORIENTED_EDGE ( 'NONE', *, *, #7697, .T. ) ;
#10406 = DIRECTION ( 'NONE',  ( 1.445602896647338917E-16, -1.000000000000000000, 0.000000000000000000 ) ) ;
#10407 = AXIS2_PLACEMENT_3D ( 'NONE', #4573, #4145, #13511 ) ;
#10408 = CARTESIAN_POINT ( 'NONE',  ( 2.789999999999999147, 13.40591150984237245, -7.739906618939567551 ) ) ;
#10409 = ORIENTED_EDGE ( 'NONE', *, *, #9410, .T. ) ;
#10410 = LINE ( 'NONE', #2457, #8555 ) ;
#10411 = ORIENTED_EDGE ( 'NONE', *, *, #6548, .T. ) ;
#10412 = B_SPLINE_CURVE_WITH_KNOTS ( 'NONE', 3,
 ( #8431, #4483, #15015, #13118, #2529, #3321 ),
 .UNSPECIFIED., .F., .F.,
 ( 4, 2, 4 ),
 ( 4.462636808902389156E-07, 0.001879885123572227514, 0.003759323983463565104 ),
 .UNSPECIFIED. ) ;
#10413 = ADVANCED_FACE ( 'NONE', ( #10767 ), #12899, .T. ) ;
#10414 = FACE_OUTER_BOUND ( 'NONE', #14848, .T. ) ;
#10415 = CARTESIAN_POINT ( 'NONE',  ( -9.403944755730119454, -4.794738323547945491, 16.99999999999999645 ) ) ;
#10416 = EDGE_CURVE ( 'NONE', #3069, #2383, #13611, .T. ) ;
#10417 = AXIS2_PLACEMENT_3D ( 'NONE', #1539, #9906, #12056 ) ;
#10418 = CARTESIAN_POINT ( 'NONE',  ( -14.40394475573011945, -10.79473832354794460, -3.794707603699265519E-15 ) ) ;
#10419 = CIRCLE ( 'NONE', #9689, 5.400000000000000355 ) ;
#10420 = DIRECTION ( 'NONE',  ( -1.000000000000000000, -0.000000000000000000, -0.000000000000000000 ) ) ;
#10421 = B_SPLINE_CURVE_WITH_KNOTS ( 'NONE', 3,
 ( #7682, #10068, #1841, #1697 ),
 .UNSPECIFIED., .F., .F.,
 ( 4, 4 ),
 ( 0.005258120783916789796, 0.005948386350302923772 ),
 .UNSPECIFIED. ) ;
#10422 = CARTESIAN_POINT ( 'NONE',  ( 13.94557569532858032, -25.06424573764405395, 7.000000000000000000 ) ) ;
#10423 = ADVANCED_FACE ( 'NONE', ( #9606 ), #2618, .T. ) ;
#10424 = CARTESIAN_POINT ( 'NONE',  ( 80.82762530298222714, -9.999999999999994671, 3.000000000000002665 ) ) ;
#10425 = EDGE_LOOP ( 'NONE', ( #6522, #5375, #6484, #9181, #5941, #2130 ) ) ;
#10426 = DIRECTION ( 'NONE',  ( -0.000000000000000000, 0.000000000000000000, 1.000000000000000000 ) ) ;
#10427 = DIRECTION ( 'NONE',  ( -0.000000000000000000, -0.000000000000000000, 1.000000000000000000 ) ) ;
#10428 = CARTESIAN_POINT ( 'NONE',  ( -14.40394475573011945, -10.79473832354794460, -3.794707603699265519E-15 ) ) ;
#10429 = AXIS2_PLACEMENT_3D ( 'NONE', #13341, #9741, #4142 ) ;
#10430 = DIRECTION ( 'NONE',  ( -1.000000000000000000, -0.000000000000000000, 0.000000000000000000 ) ) ;
#10431 = VECTOR ( 'NONE', #4017, 1000.000000000000000 ) ;
#10432 = EDGE_CURVE ( 'NONE', #3410, #11249, #5933, .T. ) ;
#10433 = ORIENTED_EDGE ( 'NONE', *, *, #589, .T. ) ;
#10434 = VECTOR ( 'NONE', #6336, 1000.000000000000000 ) ;
#10435 = CYLINDRICAL_SURFACE ( 'NONE', #13655, 13.19999999999999929 ) ;
#10436 =( NAMED_UNIT ( * ) PLANE_ANGLE_UNIT ( ) SI_UNIT ( $, .RADIAN. ) );
#10437 = ORIENTED_EDGE ( 'NONE', *, *, #13609, .T. ) ;
#10438 = ORIENTED_EDGE ( 'NONE', *, *, #10206, .T. ) ;
#10439 = DIRECTION ( 'NONE',  ( -1.000000000000000000, 0.000000000000000000, 0.000000000000000000 ) ) ;
#10440 = CARTESIAN_POINT ( 'NONE',  ( 2.764680872515353993, -5.229914364928256454, -13.68080036884353845 ) ) ;
#10441 = EDGE_LOOP ( 'NONE', ( #6112, #9669, #9030, #3218, #7510, #5290 ) ) ;
#10442 = CARTESIAN_POINT ( 'NONE',  ( 2.764680872513682885, -14.46287784598619020, 2.311161484776505404 ) ) ;
#10443 = DIRECTION ( 'NONE',  ( 0.000000000000000000, 0.000000000000000000, 1.000000000000000000 ) ) ;
#10444 = CARTESIAN_POINT ( 'NONE',  ( 14.40394475573011945, -10.79473832354794460, 5.500000000000000000 ) ) ;
#10445 = AXIS2_PLACEMENT_3D ( 'NONE', #95, #4971, #12789 ) ;
#10446 = VECTOR ( 'NONE', #9614, 1000.000000000000000 ) ;
#10447 = CIRCLE ( 'NONE', #1116, 4.000000000000000888 ) ;
#10448 = CARTESIAN_POINT ( 'NONE',  ( 2.789999999999999147, -15.74360496233394002, 18.28042085475272671 ) ) ;
#10449 = CARTESIAN_POINT ( 'NONE',  ( -16.80212006966224791, -13.74240776967763900, -3.794707603699265519E-15 ) ) ;
#10450 = EDGE_LOOP ( 'NONE', ( #14921, #7910, #11313, #13307 ) ) ;
#10451 = DIRECTION ( 'NONE',  ( 0.9021244663126475327, 0.4314758942051350465, -1.141265444721583757E-16 ) ) ;
#10452 = DIRECTION ( 'NONE',  ( -1.000000000000000000, 0.000000000000000000, -0.000000000000000000 ) ) ;
#10453 = ORIENTED_EDGE ( 'NONE', *, *, #11990, .T. ) ;
#10454 = EDGE_CURVE ( 'NONE', #10268, #4197, #11747, .T. ) ;
#10455 = AXIS2_PLACEMENT_3D ( 'NONE', #8926, #14715, #12471 ) ;
#10456 = ORIENTED_EDGE ( 'NONE', *, *, #1931, .F. ) ;
#10457 = VERTEX_POINT ( 'NONE', #5175 ) ;
#10458 = EDGE_LOOP ( 'NONE', ( #15216, #946, #15153, #2468 ) ) ;
#10459 = CARTESIAN_POINT ( 'NONE',  ( 2.236220312281012035, -12.52687487503427022, 11.41743294611070247 ) ) ;
#10460 = DIRECTION ( 'NONE',  ( 1.000000000000000000, 0.000000000000000000, 0.000000000000000000 ) ) ;
#10461 = DIRECTION ( 'NONE',  ( 0.04874958797097356245, -0.9988110320138942066, 0.000000000000000000 ) ) ;
#10462 = DIRECTION ( 'NONE',  ( -1.000000000000000000, 0.000000000000000000, 0.000000000000000000 ) ) ;
#10463 = EDGE_CURVE ( 'NONE', #9117, #5459, #79, .T. ) ;
#10464 = CIRCLE ( 'NONE', #4091, 2.447112362156698140 ) ;
#10465 = CARTESIAN_POINT ( 'NONE',  ( 2.765633920072239071, -12.59161484032927092, 21.30679549418627161 ) ) ;
#10466 = AXIS2_PLACEMENT_3D ( 'NONE', #5393, #14759, #2288 ) ;
#10467 = ORIENTED_EDGE ( 'NONE', *, *, #7905, .F. ) ;
#10468 = LINE ( 'NONE', #12690, #3542 ) ;
#10469 =( GEOMETRIC_REPRESENTATION_CONTEXT ( 3 ) GLOBAL_UNCERTAINTY_ASSIGNED_CONTEXT ( ( #3015 ) ) GLOBAL_UNIT_ASSIGNED_CONTEXT ( ( #3755, #11820, #3459 ) ) REPRESENTATION_CONTEXT ( 'NONE', 'WORKASPACE' ) );
#10470 = B_SPLINE_CURVE_WITH_KNOTS ( 'NONE', 3,
 ( #6983, #6435, #4998, #12197 ),
 .UNSPECIFIED., .F., .F.,
 ( 4, 4 ),
 ( 2.034713381942717623E-07, 0.0006887909409525219510 ),
 .UNSPECIFIED. ) ;
#10471 = FACE_OUTER_BOUND ( 'NONE', #6871, .T. ) ;
#10472 = AXIS2_PLACEMENT_3D ( 'NONE', #8839, #9847, #14541 ) ;
#10473 =( REPRESENTATION_RELATIONSHIP ('NONE','NONE', #12685, #7313 ) REPRESENTATION_RELATIONSHIP_WITH_TRANSFORMATION ( #9050 )SHAPE_REPRESENTATION_RELATIONSHIP( ) );
#10474 = EDGE_LOOP ( 'NONE', ( #14340, #10210, #9565, #10976 ) ) ;
#10475 = CARTESIAN_POINT ( 'NONE',  ( 1.039999999999997149, -4.633866840648735774, -27.68468304288263226 ) ) ;
#10476 = VECTOR ( 'NONE', #15092, 1000.000000000000000 ) ;
#10477 = CARTESIAN_POINT ( 'NONE',  ( -16.80212006966224791, -13.74240776967763900, -3.794707603699265519E-15 ) ) ;
#10478 = ORIENTED_EDGE ( 'NONE', *, *, #7758, .T. ) ;
#10479 = ORIENTED_EDGE ( 'NONE', *, *, #1979, .F. ) ;
#10480 = AXIS2_PLACEMENT_3D ( 'NONE', #1132, #9285, #10584 ) ;
#10481 = ADVANCED_FACE ( 'NONE', ( #13290, #1926 ), #1621, .F. ) ;
#10482 = DIRECTION ( 'NONE',  ( 1.000000000000000000, 0.000000000000000000, 0.000000000000000000 ) ) ;
#10483 = ORIENTED_EDGE ( 'NONE', *, *, #13966, .F. ) ;
#10484 = VECTOR ( 'NONE', #5607, 1000.000000000000000 ) ;
#10485 = CARTESIAN_POINT ( 'NONE',  ( 0.006930995026450970445, 23.92277630352802831, -5.408431875071194384 ) ) ;
#10486 = EDGE_CURVE ( 'NONE', #12007, #11663, #343, .T. ) ;
#10487 = DIRECTION ( 'NONE',  ( -1.000000000000000000, -0.000000000000000000, -0.000000000000000000 ) ) ;
#10488 = LINE ( 'NONE', #15190, #6000 ) ;
#10489 = CARTESIAN_POINT ( 'NONE',  ( 91.46153288930040048, 16.46030115554384565, 2.999999999999999112 ) ) ;
#10490 = AXIS2_PLACEMENT_3D ( 'NONE', #10959, #4988, #423 ) ;
#10491 = ORIENTED_EDGE ( 'NONE', *, *, #11745, .F. ) ;
#10492 = VECTOR ( 'NONE', #43, 1000.000000000000000 ) ;
#10493 = FACE_OUTER_BOUND ( 'NONE', #334, .T. ) ;
#10494 = CARTESIAN_POINT ( 'NONE',  ( 0.1438988480186108865, -14.59528211759996630, 5.279841123860814278 ) ) ;
#10495 =( GEOMETRIC_REPRESENTATION_CONTEXT ( 3 ) GLOBAL_UNCERTAINTY_ASSIGNED_CONTEXT ( ( #5708 ) ) GLOBAL_UNIT_ASSIGNED_CONTEXT ( ( #13836, #9086, #2307 ) ) REPRESENTATION_CONTEXT ( 'NONE', 'WORKASPACE' ) );
#10496 = ORIENTED_EDGE ( 'NONE', *, *, #11352, .F. ) ;
#10497 = EDGE_CURVE ( 'NONE', #14161, #2553, #587, .T. ) ;
#10498 = EDGE_CURVE ( 'NONE', #8078, #1582, #12857, .T. ) ;
#10499 = EDGE_CURVE ( 'NONE', #5734, #2490, #9540, .T. ) ;
#10500 = ORIENTED_EDGE ( 'NONE', *, *, #1310, .T. ) ;
#10501 = CARTESIAN_POINT ( 'NONE',  ( 0.02531912748679390063, 9.232963481057920418, -11.36963888406677725 ) ) ;
#10502 = CARTESIAN_POINT ( 'NONE',  ( 1.394999999999998685, 25.12109765559671004, -12.52377138324198214 ) ) ;
#10503 = COLOUR_RGB ( '',1.000000000000000000, 0.9490196078431372140, 0.9098039215686274384 ) ;
#10504 = FACE_OUTER_BOUND ( 'NONE', #8680, .T. ) ;
#10505 = CYLINDRICAL_SURFACE ( 'NONE', #864, 3.000000000000002665 ) ;
#10506 = CARTESIAN_POINT ( 'NONE',  ( 0.9999999999999997780, -6.008326913195983998, -0.8000000000000000444 ) ) ;
#10507 = B_SPLINE_CURVE_WITH_KNOTS ( 'NONE', 3,
 ( #13702, #6932, #9163, #9241 ),
 .UNSPECIFIED., .F., .F.,
 ( 4, 4 ),
 ( 0.005258105385878685673, 0.005948373736081384068 ),
 .UNSPECIFIED. ) ;
#10508 = AXIS2_PLACEMENT_3D ( 'NONE', #2946, #11241, #13471 ) ;
#10509 = DIRECTION ( 'NONE',  ( 0.000000000000000000, 0.000000000000000000, 1.000000000000000000 ) ) ;
#10510 = ORIENTED_EDGE ( 'NONE', *, *, #12845, .F. ) ;
#10511 = FACE_OUTER_BOUND ( 'NONE', #7678, .T. ) ;
#10512 = DIRECTION ( 'NONE',  ( -1.000000000000000000, -0.000000000000000000, -0.000000000000000000 ) ) ;
#10513 = CARTESIAN_POINT ( 'NONE',  ( 88.46153288930041469, 16.46030115554384565, 2.999999999999999112 ) ) ;
#10514 = CARTESIAN_POINT ( 'NONE',  ( 0.000000000000000000, 0.000000000000000000, 12.00000000000000000 ) ) ;
#10515 = ADVANCED_FACE ( 'NONE', ( #3999 ), #6380, .F. ) ;
#10516 = VERTEX_POINT ( 'NONE', #14765 ) ;
#10517 = CIRCLE ( 'NONE', #3885, 24.12539914357697413 ) ;
#10518 = EDGE_LOOP ( 'NONE', ( #1614, #14415, #1169, #4914, #2425, #2023, #6851 ) ) ;
#10519 = EDGE_CURVE ( 'NONE', #14952, #495, #3540, .T. ) ;
#10520 = CARTESIAN_POINT ( 'NONE',  ( 2.789999999999999147, 11.04103753892283635, -8.624777288397684316 ) ) ;
#10521 = EDGE_LOOP ( 'NONE', ( #8787, #9601, #9227, #15198, #7379, #2780, #5787, #3756 ) ) ;
#10522 = AXIS2_PLACEMENT_3D ( 'NONE', #3466, #724, #6487 ) ;
#10523 = AXIS2_PLACEMENT_3D ( 'NONE', #13329, #2807, #260 ) ;
#10524 = FACE_OUTER_BOUND ( 'NONE', #11757, .T. ) ;
#10525 = DIRECTION ( 'NONE',  ( -1.000000000000000000, 0.000000000000000000, 0.000000000000000000 ) ) ;
#10526 = LINE ( 'NONE', #13373, #5588 ) ;
#10527 = DIRECTION ( 'NONE',  ( 1.000000000000000000, 0.000000000000000000, 0.000000000000000000 ) ) ;
#10528 = DIRECTION ( 'NONE',  ( 0.000000000000000000, 0.000000000000000000, 1.000000000000000000 ) ) ;
#10529 = EDGE_CURVE ( 'NONE', #5666, #2017, #12129, .T. ) ;
#10530 = CARTESIAN_POINT ( 'NONE',  ( 1.039999999999997149, -24.89775460606822577, -12.96210679857813730 ) ) ;
#10531 = CYLINDRICAL_SURFACE ( 'NONE', #15204, 4.599999999999999645 ) ;
#10532 = ORIENTED_EDGE ( 'NONE', *, *, #3471, .T. ) ;
#10533 = CARTESIAN_POINT ( 'NONE',  ( 72.68384697807672978, 11.35494834827056110, 2.999999999999999112 ) ) ;
#10534 = AXIS2_PLACEMENT_3D ( 'NONE', #10598, #12886, #14130 ) ;
#10535 = CIRCLE ( 'NONE', #11014, 2.524999999999999023 ) ;
#10536 = AXIS2_PLACEMENT_3D ( 'NONE', #2574, #7268, #13467 ) ;
#10537 = CARTESIAN_POINT ( 'NONE',  ( 64.81187243050929681, 34.42083816749791936, 7.000000000000000000 ) ) ;
#10538 = EDGE_LOOP ( 'NONE', ( #2181, #4718, #3070, #12804 ) ) ;
#10539 =( LENGTH_UNIT ( ) NAMED_UNIT ( * ) SI_UNIT ( .MILLI., .METRE. ) );
#10540 = ORIENTED_EDGE ( 'NONE', *, *, #10056, .F. ) ;
#10541 = EDGE_LOOP ( 'NONE', ( #3609, #5579, #7198, #8374, #850, #8577, #8435, #8313 ) ) ;
#10542 = ORIENTED_EDGE ( 'NONE', *, *, #10163, .T. ) ;
#10543 = CARTESIAN_POINT ( 'NONE',  ( 0.8341307846263376069, -16.87476769693377321, 4.976600677180410770 ) ) ;
#10544 = CARTESIAN_POINT ( 'NONE',  ( 2.718184743034447237, -24.78695292654925808, 5.344212458769271201 ) ) ;
#10545 = CARTESIAN_POINT ( 'NONE',  ( -5.209999999999999964, 0.000000000000000000, 0.000000000000000000 ) ) ;
#10546 = FACE_OUTER_BOUND ( 'NONE', #12248, .T. ) ;
#10547 = CIRCLE ( 'NONE', #11993, 2.524999999999996803 ) ;
#10548 = CARTESIAN_POINT ( 'NONE',  ( 60.23740434540291488, 32.40236306526279009, 5.000000000000000888 ) ) ;
#10549 = ORIENTED_EDGE ( 'NONE', *, *, #13006, .F. ) ;
#10550 = CARTESIAN_POINT ( 'NONE',  ( -10.97587178374205941, -9.155129925568431304, -3.800000000000000266 ) ) ;
#10551 = AXIS2_PLACEMENT_3D ( 'NONE', #3318, #11311, #14779 ) ;
#10552 = VERTEX_POINT ( 'NONE', #10990 ) ;
#10553 = CARTESIAN_POINT ( 'NONE',  ( 1.960886852992457241, 24.44424927289185945, 12.96989951879416125 ) ) ;
#10554 = DIRECTION ( 'NONE',  ( 1.000000000000000000, 0.000000000000000000, 0.000000000000000000 ) ) ;
#10555 = EDGE_CURVE ( 'NONE', #13089, #10675, #8906, .T. ) ;
#10556 = ORIENTED_EDGE ( 'NONE', *, *, #11882, .F. ) ;
#10557 = ORIENTED_EDGE ( 'NONE', *, *, #2847, .T. ) ;
#10558 = FACE_OUTER_BOUND ( 'NONE', #1060, .T. ) ;
#10559 = B_SPLINE_CURVE_WITH_KNOTS ( 'NONE', 3,
 ( #11231, #4175, #9781, #14480 ),
 .UNSPECIFIED., .F., .F.,
 ( 4, 4 ),
 ( 2.451234579310871045E-07, 0.0006917187676826522767 ),
 .UNSPECIFIED. ) ;
#10560 = ORIENTED_EDGE ( 'NONE', *, *, #13952, .T. ) ;
#10561 = LINE ( 'NONE', #77, #11887 ) ;
#10562 = CARTESIAN_POINT ( 'NONE',  ( 5.999999999999999112, 7.347880794884118750E-16, 5.500000000000000000 ) ) ;
#10563 = ADVANCED_FACE ( 'NONE', ( #11064 ), #3063, .T. ) ;
#10564 = LINE ( 'NONE', #8325, #3774 ) ;
#10565 = CARTESIAN_POINT ( 'NONE',  ( 98.48580539929344013, 0.9022481406819604643, 7.000000000000000000 ) ) ;
#10566 = ORIENTED_EDGE ( 'NONE', *, *, #4999, .T. ) ;
#10567 = FACE_OUTER_BOUND ( 'NONE', #4346, .T. ) ;
#10568 = EDGE_CURVE ( 'NONE', #12453, #5145, #13363, .T. ) ;
#10569 = CARTESIAN_POINT ( 'NONE',  ( 0.000000000000000000, 1.621424371464993087E-13, -12.95481323787947936 ) ) ;
#10570 = EDGE_LOOP ( 'NONE', ( #7029, #9710, #13822, #5834 ) ) ;
#10571 = EDGE_CURVE ( 'NONE', #6770, #11883, #11554, .T. ) ;
#10572 = EDGE_LOOP ( 'NONE', ( #788, #13664, #562, #7051 ) ) ;
#10573 = CARTESIAN_POINT ( 'NONE',  ( 0.02531912748464587928, -5.229914364928447412, 13.68080036884346917 ) ) ;
#10574 = CARTESIAN_POINT ( 'NONE',  ( -7.723595606797438030E-14, -23.69897269326674305, -5.456611084822102775 ) ) ;
#10575 = CARTESIAN_POINT ( 'NONE',  ( 0.000000000000000000, -24.34211360614305875, 7.909232158574721616 ) ) ;
#10576 = LINE ( 'NONE', #2349, #13113 ) ;
#10577 = DIRECTION ( 'NONE',  ( 0.000000000000000000, 0.000000000000000000, -1.000000000000000000 ) ) ;
#10578 = B_SPLINE_CURVE_WITH_KNOTS ( 'NONE', 3,
 ( #12008, #10858, #5197, #317, #9711, #398 ),
 .UNSPECIFIED., .F., .F.,
 ( 4, 2, 4 ),
 ( 2.132675795045763710E-07, 0.001878604073277002169, 0.003756994878974500001 ),
 .UNSPECIFIED. ) ;
#10579 = CARTESIAN_POINT ( 'NONE',  ( 1.394999999999999574, 17.39253030560841751, -4.458161950358562109 ) ) ;
#10580 = ADVANCED_FACE ( 'NONE', ( #2927 ), #7683, .T. ) ;
#10581 = ORIENTED_EDGE ( 'NONE', *, *, #7322, .T. ) ;
#10582 = DIRECTION ( 'NONE',  ( -1.000000000000000000, 0.000000000000000000, 0.000000000000000000 ) ) ;
#10583 = CARTESIAN_POINT ( 'NONE',  ( 1.039999999999996483, -12.96210679857803783, 24.89775460606827551 ) ) ;
#10584 = DIRECTION ( 'NONE',  ( 0.000000000000000000, 0.000000000000000000, 1.000000000000000000 ) ) ;
#10585 = CARTESIAN_POINT ( 'NONE',  ( 2.789999999999999147, 2.680914349914567470E-13, -25.59481291497571220 ) ) ;
#10586 = EDGE_LOOP ( 'NONE', ( #4047, #405, #5716, #5758 ) ) ;
#10587 = ORIENTED_EDGE ( 'NONE', *, *, #646, .T. ) ;
#10588 = SURFACE_STYLE_USAGE ( .BOTH. , #3958 ) ;
#10589 = ADVANCED_FACE ( 'NONE', ( #6454 ), #13593, .T. ) ;
#10590 = ORIENTED_EDGE ( 'NONE', *, *, #9288, .F. ) ;
#10591 = CYLINDRICAL_SURFACE ( 'NONE', #14422, 6.000000000000000000 ) ;
#10592 = DIRECTION ( 'NONE',  ( 0.000000000000000000, 0.000000000000000000, 1.000000000000000000 ) ) ;
#10593 = LINE ( 'NONE', #4756, #13179 ) ;
#10594 = CYLINDRICAL_SURFACE ( 'NONE', #14363, 28.06981291497571362 ) ;
#10595 = CARTESIAN_POINT ( 'NONE',  ( 2.789679245949058917, 20.70663861606308487, -12.51925356660738053 ) ) ;
#10596 = EDGE_CURVE ( 'NONE', #14085, #5202, #7545, .T. ) ;
#10597 = CYLINDRICAL_SURFACE ( 'NONE', #12265, 4.599999999999999645 ) ;
#10598 = CARTESIAN_POINT ( 'NONE',  ( -5.209999999999999964, 0.000000000000000000, 0.000000000000000000 ) ) ;
#10599 = EDGE_CURVE ( 'NONE', #3713, #3154, #3159, .T. ) ;
#10600 = EDGE_CURVE ( 'NONE', #1772, #2773, #7915, .T. ) ;
#10601 = VERTEX_POINT ( 'NONE', #2225 ) ;
#10602 = CARTESIAN_POINT ( 'NONE',  ( -14.40394475573011945, -10.79473832354794283, -3.000000000000000000 ) ) ;
#10603 = DIRECTION ( 'NONE',  ( 0.000000000000000000, 0.000000000000000000, 1.000000000000000000 ) ) ;
#10604 = ORIENTED_EDGE ( 'NONE', *, *, #6634, .T. ) ;
#10605 = ORIENTED_EDGE ( 'NONE', *, *, #1712, .F. ) ;
#10606 = ORIENTED_EDGE ( 'NONE', *, *, #14570, .T. ) ;
#10607 = VERTEX_POINT ( 'NONE', #15143 ) ;
#10608 = DIRECTION ( 'NONE',  ( 1.000000000000000000, 0.000000000000000000, 0.000000000000000000 ) ) ;
#10609 = DIRECTION ( 'NONE',  ( -1.000000000000000000, -0.000000000000000000, -0.000000000000000000 ) ) ;
#10610 = CIRCLE ( 'NONE', #8151, 28.06981291497571007 ) ;
#10611 = DIRECTION ( 'NONE',  ( 1.000000000000000000, 0.000000000000000000, -0.000000000000000000 ) ) ;
#10612 = DIRECTION ( 'NONE',  ( 0.000000000000000000, -0.000000000000000000, -1.000000000000000000 ) ) ;
#10613 = EDGE_CURVE ( 'NONE', #9942, #7028, #6618, .T. ) ;
#10614 = EDGE_CURVE ( 'NONE', #6170, #13370, #13824, .T. ) ;
#10615 = CARTESIAN_POINT ( 'NONE',  ( 1.000000000000000000, -6.008326913195983998, 0.000000000000000000 ) ) ;
#10616 = B_SPLINE_CURVE_WITH_KNOTS ( 'NONE', 3,
 ( #5706, #10315, #15163, #8152, #6928, #11604, #1083, #4639 ),
 .UNSPECIFIED., .F., .F.,
 ( 4, 2, 2, 4 ),
 ( 4.663089536289470154E-07, 0.001898630414085403445, 0.002847712466651290599, 0.003796794519217177970 ),
 .UNSPECIFIED. ) ;
#10617 = EDGE_CURVE ( 'NONE', #9825, #9957, #10296, .T. ) ;
#10618 = VERTEX_POINT ( 'NONE', #3379 ) ;
#10619 = DIRECTION ( 'NONE',  ( -1.000000000000000000, -0.000000000000000000, -0.000000000000000000 ) ) ;
#10620 = AXIS2_PLACEMENT_3D ( 'NONE', #11045, #7374, #6136 ) ;
#10621 = ADVANCED_FACE ( 'NONE', ( #6685 ), #11365, .F. ) ;
#10622 = ORIENTED_EDGE ( 'NONE', *, *, #6937, .T. ) ;
#10623 = FACE_OUTER_BOUND ( 'NONE', #7457, .T. ) ;
#10624 = CARTESIAN_POINT ( 'NONE',  ( 8.961831343790189308, 9.104486995144791095, -130.1575142076926852 ) ) ;
#10625 = VERTEX_POINT ( 'NONE', #4303 ) ;
#10626 = ORIENTED_EDGE ( 'NONE', *, *, #7015, .F. ) ;
#10627 = CARTESIAN_POINT ( 'NONE',  ( 2.789999999999999147, 23.48180575137730131, 5.535312321042802353 ) ) ;
#10628 = EDGE_LOOP ( 'NONE', ( #2828, #5502, #5142, #12992 ) ) ;
#10629 = CARTESIAN_POINT ( 'NONE',  ( 0.02531912748631424959, 14.46287784598617243, 2.311161484776605324 ) ) ;
#10630 = CARTESIAN_POINT ( 'NONE',  ( 1.749999999999998002, -20.02152543075360214, 19.67366047555523068 ) ) ;
#10631 = DIRECTION ( 'NONE',  ( -0.000000000000000000, -0.000000000000000000, 1.000000000000000000 ) ) ;
#10632 = CARTESIAN_POINT ( 'NONE',  ( -20.63749999999999929, 0.000000000000000000, 0.000000000000000000 ) ) ;
#10633 = ORIENTED_EDGE ( 'NONE', *, *, #5649, .F. ) ;
#10634 = DIRECTION ( 'NONE',  ( -1.000000000000000000, 0.000000000000000000, 0.000000000000000000 ) ) ;
#10635 = CARTESIAN_POINT ( 'NONE',  ( 2.789999999999999147, 18.55949924794892780, 16.37294372382865504 ) ) ;
#10636 = ORIENTED_EDGE ( 'NONE', *, *, #14073, .F. ) ;
#10637 = ORIENTED_EDGE ( 'NONE', *, *, #11336, .T. ) ;
#10638 = DIRECTION ( 'NONE',  ( -1.000000000000000000, -0.000000000000000000, -0.000000000000000000 ) ) ;
#10639 = LINE ( 'NONE', #4815, #14950 ) ;
#10640 = AXIS2_PLACEMENT_3D ( 'NONE', #11960, #428, #2682 ) ;
#10641 = DIRECTION ( 'NONE',  ( -1.000000000000000000, -0.000000000000000000, 0.000000000000000000 ) ) ;
#10642 = DIRECTION ( 'NONE',  ( 0.000000000000000000, 0.000000000000000000, 1.000000000000000000 ) ) ;
#10643 = CARTESIAN_POINT ( 'NONE',  ( 2.718131885465892239, -16.91241718341984779, -18.89333555428573774 ) ) ;
#10644 = EDGE_CURVE ( 'NONE', #516, #8949, #7958, .T. ) ;
#10645 = PLANE ( 'NONE',  #9332 ) ;
#10646 = ORIENTED_EDGE ( 'NONE', *, *, #3261, .F. ) ;
#10647 = CARTESIAN_POINT ( 'NONE',  ( 2.765633920072235519, 18.55949924794892780, 16.37294372382865504 ) ) ;
#10648 = CIRCLE ( 'NONE', #3777, 7.000000000000000000 ) ;
#10649 = CARTESIAN_POINT ( 'NONE',  ( 88.46153288930041469, 16.46030115554384565, 7.000000000000000000 ) ) ;
#10650 = CARTESIAN_POINT ( 'NONE',  ( 0.000000000000000000, 1.948757464274177842, 13.87420763704361981 ) ) ;
#10651 = CARTESIAN_POINT ( 'NONE',  ( -0.1717365941144614327, -6.008326913195983998, 0.000000000000000000 ) ) ;
#10652 = ORIENTED_EDGE ( 'NONE', *, *, #12475, .T. ) ;
#10653 = ORIENTED_EDGE ( 'NONE', *, *, #1459, .F. ) ;
#10654 = AXIS2_PLACEMENT_3D ( 'NONE', #7616, #12292, #1766 ) ;
#10655 = AXIS2_PLACEMENT_3D ( 'NONE', #3023, #13705, #7708 ) ;
#10656 = ORIENTED_EDGE ( 'NONE', *, *, #9245, .T. ) ;
#10657 = VECTOR ( 'NONE', #4239, 1000.000000000000000 ) ;
#10658 = CARTESIAN_POINT ( 'NONE',  ( 8.000000000000000000, 0.000000000000000000, 0.000000000000000000 ) ) ;
#10659 = CARTESIAN_POINT ( 'NONE',  ( -7.688810570594222860E-14, -5.456611084822025504, 23.69897269326675016 ) ) ;
#10660 = CARTESIAN_POINT ( 'NONE',  ( 1.749999999999998002, -27.76164181293049182, -4.147968289691579713 ) ) ;
#10661 = DIRECTION ( 'NONE',  ( 1.000000000000000000, 0.000000000000000000, 0.000000000000000000 ) ) ;
#10662 = DIRECTION ( 'NONE',  ( 1.000000000000000000, 0.000000000000000000, 0.000000000000000000 ) ) ;
#10663 = CARTESIAN_POINT ( 'NONE',  ( 2.765633920072235519, 24.15498966839970052, -5.391175441198366336 ) ) ;
#10664 = ORIENTED_EDGE ( 'NONE', *, *, #2429, .F. ) ;
#10665 = PLANE ( 'NONE',  #4682 ) ;
#10666 = FACE_OUTER_BOUND ( 'NONE', #14386, .T. ) ;
#10667 = CIRCLE ( 'NONE', #14114, 28.06981291497571362 ) ;
#10668 = AXIS2_PLACEMENT_3D ( 'NONE', #10927, #12238, #6244 ) ;
#10669 = EDGE_LOOP ( 'NONE', ( #2752, #14315, #1659, #14773 ) ) ;
#10670 = FACE_OUTER_BOUND ( 'NONE', #11596, .T. ) ;
#10671 = CARTESIAN_POINT ( 'NONE',  ( 1.039999999999996039, -12.83329210556840394, 12.55714665599982816 ) ) ;
#10672 = VECTOR ( 'NONE', #11320, 1000.000000000000000 ) ;
#10673 = EDGE_CURVE ( 'NONE', #10607, #7692, #10362, .T. ) ;
#10674 = DIRECTION ( 'NONE',  ( 0.000000000000000000, 0.000000000000000000, 1.000000000000000000 ) ) ;
#10675 = VERTEX_POINT ( 'NONE', #9072 ) ;
#10676 = B_SPLINE_CURVE_WITH_KNOTS ( 'NONE', 3,
 ( #1330, #6026, #9401, #12713, #15109, #5733, #4666, #171 ),
 .UNSPECIFIED., .F., .F.,
 ( 4, 2, 2, 4 ),
 ( 2.154797737796238865E-07, 0.001895231411415137677, 0.002842739377235819348, 0.003790247343056501236 ),
 .UNSPECIFIED. ) ;
#10677 = SURFACE_STYLE_FILL_AREA ( #8143 ) ;
#10678 = CARTESIAN_POINT ( 'NONE',  ( 80.00000000000000000, 0.000000000000000000, -130.1575142076926852 ) ) ;
#10679 = ORIENTED_EDGE ( 'NONE', *, *, #9063, .T. ) ;
#10680 = VERTEX_POINT ( 'NONE', #836 ) ;
#10681 = ORIENTED_EDGE ( 'NONE', *, *, #2042, .T. ) ;
#10682 = FACE_BOUND ( 'NONE', #11318, .T. ) ;
#10683 = VECTOR ( 'NONE', #14165, 1000.000000000000114 ) ;
#10684 = FACE_OUTER_BOUND ( 'NONE', #1211, .T. ) ;
#10685 = ADVANCED_FACE ( 'NONE', ( #2002 ), #13676, .T. ) ;
#10686 = EDGE_CURVE ( 'NONE', #10625, #2957, #2556, .T. ) ;
#10687 = AXIS2_PLACEMENT_3D ( 'NONE', #3475, #3191, #11688 ) ;
#10688 = DIRECTION ( 'NONE',  ( 0.000000000000000000, 0.000000000000000000, 1.000000000000000000 ) ) ;
#10689 = DIRECTION ( 'NONE',  ( 0.000000000000000000, 0.000000000000000000, -1.000000000000000000 ) ) ;
#10690 = CARTESIAN_POINT ( 'NONE',  ( 0.02531912748464761401, -2.311161484776455222, -14.46287784598619908 ) ) ;
#10691 = EDGE_LOOP ( 'NONE', ( #619, #4246, #9, #7920, #2718, #662, #5184, #9736, #4380, #7633, #13809, #12823, #8824, #4504, #8900, #13993 ) ) ;
#10692 = CARTESIAN_POINT ( 'NONE',  ( 2.789999999999999147, 1.991882183130294637, 24.04302995059966364 ) ) ;
#10693 = AXIS2_PLACEMENT_3D ( 'NONE', #14684, #4154, #8827 ) ;
#10694 = CIRCLE ( 'NONE', #8464, 4.999999999999997335 ) ;
#10695 = EDGE_CURVE ( 'NONE', #11429, #11249, #4538, .T. ) ;
#10696 = EDGE_CURVE ( 'NONE', #9402, #12714, #9142, .T. ) ;
#10697 = ORIENTED_EDGE ( 'NONE', *, *, #1696, .T. ) ;
#10698 = DIRECTION ( 'NONE',  ( 0.000000000000000000, 0.000000000000000000, 1.000000000000000000 ) ) ;
#10699 = PRODUCT ( 'plate 2', 'plate 2', '', ( #666 ) ) ;
#10700 = CARTESIAN_POINT ( 'NONE',  ( 0.5431871499410859672, -16.16568790143438150, -5.154374911959082262 ) ) ;
#10701 = EDGE_CURVE ( 'NONE', #12700, #6090, #13755, .T. ) ;
#10702 = ORIENTED_EDGE ( 'NONE', *, *, #10233, .T. ) ;
#10703 = ORIENTED_EDGE ( 'NONE', *, *, #227, .F. ) ;
#10704 = VECTOR ( 'NONE', #760, 1000.000000000000114 ) ;
#10705 = DIRECTION ( 'NONE',  ( -1.000000000000000000, 0.000000000000000000, 0.000000000000000000 ) ) ;
#10706 = ADVANCED_FACE ( 'NONE', ( #8134 ), #1585, .T. ) ;
#10707 = ORIENTED_EDGE ( 'NONE', *, *, #2116, .F. ) ;
#10708 = DIRECTION ( 'NONE',  ( 0.000000000000000000, 0.000000000000000000, 1.000000000000000000 ) ) ;
#10709 = DIRECTION ( 'NONE',  ( 0.000000000000000000, 0.000000000000000000, -1.000000000000000000 ) ) ;
#10710 = CIRCLE ( 'NONE', #11679, 24.12539914357697768 ) ;
#10711 = DIRECTION ( 'NONE',  ( 1.000000000000000000, 0.000000000000000000, 0.000000000000000000 ) ) ;
#10712 = ORIENTED_EDGE ( 'NONE', *, *, #1592, .T. ) ;
#10713 = AXIS2_PLACEMENT_3D ( 'NONE', #6179, #10861, #320 ) ;
#10714 = CARTESIAN_POINT ( 'NONE',  ( 61.44848940674400239, 29.65768221419895667, 4.000000000000000000 ) ) ;
#10715 = DIRECTION ( 'NONE',  ( 1.000000000000000000, 0.000000000000000000, -0.000000000000000000 ) ) ;
#10716 = STYLED_ITEM ( 'NONE', ( #2235 ), #13135 ) ;
#10717 = VECTOR ( 'NONE', #9631, 1000.000000000000114 ) ;
#10718 = ORIENTED_EDGE ( 'NONE', *, *, #12144, .F. ) ;
#10719 = DIRECTION ( 'NONE',  ( 0.000000000000000000, 0.000000000000000000, 1.000000000000000000 ) ) ;
#10720 = ORIENTED_EDGE ( 'NONE', *, *, #3944, .T. ) ;
#10721 = ORIENTED_EDGE ( 'NONE', *, *, #8349, .F. ) ;
#10722 = CARTESIAN_POINT ( 'NONE',  ( 0.007349557670559650827, 9.045126717605935340, -11.23191127083853935 ) ) ;
#10723 = LINE ( 'NONE', #1337, #13949 ) ;
#10724 = AXIS2_PLACEMENT_3D ( 'NONE', #6217, #10060, #3919 ) ;
#10725 = DIRECTION ( 'NONE',  ( 0.000000000000000000, 0.000000000000000000, 1.000000000000000000 ) ) ;
#10726 = DIRECTION ( 'NONE',  ( 0.000000000000000000, 0.000000000000000000, -1.000000000000000000 ) ) ;
#10727 = CARTESIAN_POINT ( 'NONE',  ( -16.14082873121598993, -7.414910804916202913, -3.800000000000000266 ) ) ;
#10728 = CARTESIAN_POINT ( 'NONE',  ( 0.001869172971454433714, -20.90869469097853894, -12.51925356660784594 ) ) ;
#10729 = VERTEX_POINT ( 'NONE', #5619 ) ;
#10730 = DIRECTION ( 'NONE',  ( -1.000000000000000000, 0.000000000000000000, 0.000000000000000000 ) ) ;
#10731 = CARTESIAN_POINT ( 'NONE',  ( 1.394999999999999574, -4.458161950358622505, 17.39253030560840330 ) ) ;
#10732 = AXIS2_PLACEMENT_3D ( 'NONE', #4777, #8443, #11759 ) ;
#10733 = CARTESIAN_POINT ( 'NONE',  ( 0.1882238782932344201, 17.47009390565490605, 19.18368891937496556 ) ) ;
#10734 = CARTESIAN_POINT ( 'NONE',  ( 2.790000000000077307, 22.38018801136476554, 9.515416771311276278 ) ) ;
#10735 = AXIS2_PLACEMENT_3D ( 'NONE', #13728, #657, #10186 ) ;
#10736 = ORIENTED_EDGE ( 'NONE', *, *, #13498, .F. ) ;
#10737 = ORIENTED_EDGE ( 'NONE', *, *, #14618, .F. ) ;
#10738 = ORIENTED_EDGE ( 'NONE', *, *, #1696, .F. ) ;
#10739 = AXIS2_PLACEMENT_3D ( 'NONE', #10418, #13960, #12788 ) ;
#10740 = DIRECTION ( 'NONE',  ( -1.000000000000000000, 0.000000000000000000, 0.000000000000000000 ) ) ;
#10741 = CARTESIAN_POINT ( 'NONE',  ( 2.765633920072236407, 2.336989772644613161, -24.63872515616080250 ) ) ;
#10742 = EDGE_CURVE ( 'NONE', #11509, #1482, #4462, .T. ) ;
#10743 = AXIS2_PLACEMENT_3D ( 'NONE', #9656, #8277, #6977 ) ;
#10744 = CARTESIAN_POINT ( 'NONE',  ( 0.000000000000000000, 0.000000000000000000, 0.000000000000000000 ) ) ;
#10745 = CARTESIAN_POINT ( 'NONE',  ( 2.789999999999999147, 4.595504208220227760, -14.19996452731184178 ) ) ;
#10746 = DIRECTION ( 'NONE',  ( 5.480158469902919838E-17, -1.051478716308701618E-16, 1.000000000000000000 ) ) ;
#10747 = CYLINDRICAL_SURFACE ( 'NONE', #6451, 8.400000000000000355 ) ;
#10748 = ORIENTED_EDGE ( 'NONE', *, *, #1310, .F. ) ;
#10749 = CYLINDRICAL_SURFACE ( 'NONE', #5657, 31.62277660168379256 ) ;
#10750 = CARTESIAN_POINT ( 'NONE',  ( -1.000000000000000222, -4.808326913195983821, -0.8000000000000000444 ) ) ;
#10751 = VERTEX_POINT ( 'NONE', #12809 ) ;
#10752 = CARTESIAN_POINT ( 'NONE',  ( 85.79342132543153809, 17.83186255874426962, 2.999999999999999112 ) ) ;
#10753 = DIRECTION ( 'NONE',  ( -0.000000000000000000, -0.000000000000000000, -1.000000000000000000 ) ) ;
#10754 =( GEOMETRIC_REPRESENTATION_CONTEXT ( 3 ) GLOBAL_UNCERTAINTY_ASSIGNED_CONTEXT ( ( #609 ) ) GLOBAL_UNIT_ASSIGNED_CONTEXT ( ( #10866, #1567, #1729 ) ) REPRESENTATION_CONTEXT ( 'NONE', 'WORKASPACE' ) );
#10755 = EDGE_CURVE ( 'NONE', #4429, #15084, #5766, .T. ) ;
#10756 = EDGE_LOOP ( 'NONE', ( #11303, #8317, #5773, #12125 ) ) ;
#10757 = CIRCLE ( 'NONE', #185, 4.000000000000003553 ) ;
#10758 = VECTOR ( 'NONE', #251, 1000.000000000000000 ) ;
#10759 = EDGE_CURVE ( 'NONE', #12711, #11373, #12379, .T. ) ;
#10760 = VERTEX_POINT ( 'NONE', #1220 ) ;
#10761 = ORIENTED_EDGE ( 'NONE', *, *, #5076, .T. ) ;
#10762 = ORIENTED_EDGE ( 'NONE', *, *, #11712, .T. ) ;
#10763 = CARTESIAN_POINT ( 'NONE',  ( 2.789999999999999147, 15.04425356660790136, -18.18163861606255338 ) ) ;
#10764 = CARTESIAN_POINT ( 'NONE',  ( 0.02531912748464761401, -2.311161484776455222, -14.46287784598619908 ) ) ;
#10765 = ADVANCED_FACE ( 'NONE', ( #7061 ), #12963, .T. ) ;
#10766 = CARTESIAN_POINT ( 'NONE',  ( 0.000000000000000000, 0.000000000000000000, 4.500000000000000888 ) ) ;
#10767 = FACE_OUTER_BOUND ( 'NONE', #5129, .T. ) ;
#10768 = CARTESIAN_POINT ( 'NONE',  ( 2.718131885465890463, 18.89333555428578748, -16.91241718341978029 ) ) ;
#10769 = APPLICATION_CONTEXT ( 'automotive_design' ) ;
#10770 = CIRCLE ( 'NONE', #9502, 3.000000000000000888 ) ;
#10771 = ORIENTED_EDGE ( 'NONE', *, *, #13704, .T. ) ;
#10772 = CARTESIAN_POINT ( 'NONE',  ( 1.039999999999997149, -4.633866840648735774, -27.68468304288263226 ) ) ;
#10773 = EDGE_CURVE ( 'NONE', #10133, #5736, #2389, .T. ) ;
#10774 = EDGE_CURVE ( 'NONE', #8517, #9447, #3782, .T. ) ;
#10775 = TOROIDAL_SURFACE ( 'NONE', #9060, 24.12539914357697413, 8.000000000000000000 ) ;
#10776 = VERTEX_POINT ( 'NONE', #44 ) ;
#10777 = AXIS2_PLACEMENT_3D ( 'NONE', #4283, #8963, #13654 ) ;
#10778 = CARTESIAN_POINT ( 'NONE',  ( 2.789999999999999147, -22.25075486061731667, -9.324097380959683434 ) ) ;
#10779 = DIRECTION ( 'NONE',  ( -1.000000000000000000, 0.000000000000000000, -0.000000000000000000 ) ) ;
#10780 = ORIENTED_EDGE ( 'NONE', *, *, #12004, .F. ) ;
#10781 = ORIENTED_EDGE ( 'NONE', *, *, #2673, .F. ) ;
#10782 = CYLINDRICAL_SURFACE ( 'NONE', #8720, 2.999999999999988898 ) ;
#10783 = ADVANCED_FACE ( 'NONE', ( #9589 ), #10594, .T. ) ;
#10784 = EDGE_LOOP ( 'NONE', ( #1837, #13018, #4809, #4772 ) ) ;
#10785 = CARTESIAN_POINT ( 'NONE',  ( 20.40394475573011590, -10.79473832354794460, 5.500000000000001776 ) ) ;
#10786 = CARTESIAN_POINT ( 'NONE',  ( 8.961831343790189308, 9.104486995144789319, 7.000000000000000000 ) ) ;
#10787 = EDGE_CURVE ( 'NONE', #13045, #484, #4416, .T. ) ;
#10788 = EDGE_CURVE ( 'NONE', #12264, #3700, #4757, .T. ) ;
#10789 = DIRECTION ( 'NONE',  ( 1.000000000000000000, 0.000000000000000000, 0.000000000000000000 ) ) ;
#10790 = DIRECTION ( 'NONE',  ( 0.000000000000000000, 0.000000000000000000, 1.000000000000000000 ) ) ;
#10791 = ORIENTED_EDGE ( 'NONE', *, *, #9951, .F. ) ;
#10792 = DIRECTION ( 'NONE',  ( -0.9728364810787193395, -0.2314933715733012709, -0.000000000000000000 ) ) ;
#10793 = DIRECTION ( 'NONE',  ( 0.000000000000000000, 0.000000000000000000, 1.000000000000000000 ) ) ;
#10794 = ORIENTED_EDGE ( 'NONE', *, *, #15016, .F. ) ;
#10795 = CARTESIAN_POINT ( 'NONE',  ( 0.02531912748679129854, 11.36963888406687317, 9.232963481057801403 ) ) ;
#10796 = VERTEX_POINT ( 'NONE', #1446 ) ;
#10797 = ORIENTED_EDGE ( 'NONE', *, *, #11693, .F. ) ;
#10798 = DIRECTION ( 'NONE',  ( 1.000000000000000000, 0.000000000000000000, 0.000000000000000000 ) ) ;
#10799 = CARTESIAN_POINT ( 'NONE',  ( 0.000000000000000000, 0.000000000000000000, 4.000000000000000000 ) ) ;
#10800 = SURFACE_SIDE_STYLE ('',( #5131 ) ) ;
#10801 = DIRECTION ( 'NONE',  ( 1.000000000000000000, -6.245004513516508695E-15, 0.000000000000000000 ) ) ;
#10802 = CARTESIAN_POINT ( 'NONE',  ( -19.40394475573011590, -4.794738323547945491, 12.00000000000000000 ) ) ;
#10803 = CARTESIAN_POINT ( 'NONE',  ( 0.0003207540509381473352, -20.70663861606275447, -12.51925356660783528 ) ) ;
#10804 = EDGE_LOOP ( 'NONE', ( #13149, #3811, #13415, #1153 ) ) ;
#10805 = CARTESIAN_POINT ( 'NONE',  ( 0.000000000000000000, 0.000000000000000000, 0.000000000000000000 ) ) ;
#10806 = DIRECTION ( 'NONE',  ( -1.000000000000000000, -0.000000000000000000, -0.000000000000000000 ) ) ;
#10807 = CARTESIAN_POINT ( 'NONE',  ( 2.764680872513682441, -2.311161484776455222, -14.46287784598619908 ) ) ;
#10808 = DIRECTION ( 'NONE',  ( -1.000000000000000000, -0.000000000000000000, -0.000000000000000000 ) ) ;
#10809 = VERTEX_POINT ( 'NONE', #10816 ) ;
#10810 = ORIENTED_EDGE ( 'NONE', *, *, #11076, .T. ) ;
#10811 = EDGE_CURVE ( 'NONE', #12279, #2475, #4049, .T. ) ;
#10812 = ORIENTED_EDGE ( 'NONE', *, *, #7802, .F. ) ;
#10813 = CARTESIAN_POINT ( 'NONE',  ( -14.40394475573012301, -4.794738323547945491, 13.99999999999999645 ) ) ;
#10814 = DIRECTION ( 'NONE',  ( -0.9148936170212769170, -0.4036950204470268755, 0.000000000000000000 ) ) ;
#10815 = LINE ( 'NONE', #3514, #9498 ) ;
#10816 = CARTESIAN_POINT ( 'NONE',  ( 1.749999999999999778, 12.55714665600005020, -12.83329210556818545 ) ) ;
#10817 = DIRECTION ( 'NONE',  ( 1.000000000000000000, 0.000000000000000000, 0.000000000000000000 ) ) ;
#10818 = DIRECTION ( 'NONE',  ( -1.000000000000000000, 0.000000000000000000, 0.000000000000000000 ) ) ;
#10819 = EDGE_LOOP ( 'NONE', ( #15069, #6148, #9961, #6407 ) ) ;
#10820 = FACE_OUTER_BOUND ( 'NONE', #10628, .T. ) ;
#10821 = CARTESIAN_POINT ( 'NONE',  ( 2.789999999999999147, 11.04103753892271556, 8.624777288397840636 ) ) ;
#10822 = ORIENTED_EDGE ( 'NONE', *, *, #2155, .F. ) ;
#10823 = CYLINDRICAL_SURFACE ( 'NONE', #1429, 4.000000000000000000 ) ;
#10824 = DIRECTION ( 'NONE',  ( 0.000000000000000000, 1.000000000000000000, 1.030528797609984825E-14 ) ) ;
#10825 = FILL_AREA_STYLE ('',( #127 ) ) ;
#10826 = EDGE_CURVE ( 'NONE', #11452, #7572, #757, .T. ) ;
#10827 = VERTEX_POINT ( 'NONE', #14124 ) ;
#10828 = B_SPLINE_CURVE_WITH_KNOTS ( 'NONE', 3,
 ( #12924, #16, #7103, #9178, #11778, #13863 ),
 .UNSPECIFIED., .F., .F.,
 ( 4, 2, 4 ),
 ( 4.462636882221166670E-07, 0.001879885203074802827, 0.003759324142461383488 ),
 .UNSPECIFIED. ) ;
#10829 = DIRECTION ( 'NONE',  ( 0.000000000000000000, 0.000000000000000000, -1.000000000000000000 ) ) ;
#10830 = EDGE_LOOP ( 'NONE', ( #36, #11446 ) ) ;
#10831 = ORIENTED_EDGE ( 'NONE', *, *, #9004, .T. ) ;
#10832 = VERTEX_POINT ( 'NONE', #1516 ) ;
#10833 = CARTESIAN_POINT ( 'NONE',  ( 2.789999999999999147, -9.999777909380009433, 11.07980565117276761 ) ) ;
#10834 = CARTESIAN_POINT ( 'NONE',  ( 0.07473581742173487918, -5.299647274067002201, -14.31752701692942153 ) ) ;
#10835 = CARTESIAN_POINT ( 'NONE',  ( 0.7795480803411078963, 16.99607982911242132, 4.029281904976690143 ) ) ;
#10836 = CARTESIAN_POINT ( 'NONE',  ( 0.000000000000000000, 0.000000000000000000, 5.500000000000000000 ) ) ;
#10837 = CARTESIAN_POINT ( 'NONE',  ( -14.40394475573011945, -10.79473832354794460, -3.794707603699265519E-15 ) ) ;
#10838 = EDGE_CURVE ( 'NONE', #3736, #13302, #6058, .T. ) ;
#10839 = DIRECTION ( 'NONE',  ( 0.000000000000000000, 0.000000000000000000, 1.000000000000000000 ) ) ;
#10840 = EDGE_CURVE ( 'NONE', #10809, #1007, #11406, .T. ) ;
#10841 = ORIENTED_EDGE ( 'NONE', *, *, #11277, .F. ) ;
#10842 = CARTESIAN_POINT ( 'NONE',  ( -4.000000000000000888, 0.000000000000000000, 10.00000000000000000 ) ) ;
#10843 = CIRCLE ( 'NONE', #13041, 6.000000000000000000 ) ;
#10844 = ORIENTED_EDGE ( 'NONE', *, *, #11140, .F. ) ;
#10845 = ORIENTED_EDGE ( 'NONE', *, *, #8169, .F. ) ;
#10846 = DIRECTION ( 'NONE',  ( 1.000000000000000000, 0.000000000000000000, 0.000000000000000000 ) ) ;
#10847 = DIRECTION ( 'NONE',  ( -1.000000000000000000, 0.000000000000000000, 0.000000000000000000 ) ) ;
#10848 = VERTEX_POINT ( 'NONE', #273 ) ;
#10849 = DIRECTION ( 'NONE',  ( 0.000000000000000000, 0.000000000000000000, 1.000000000000000000 ) ) ;
#10850 = EDGE_LOOP ( 'NONE', ( #4350, #4830, #7694, #2145, #5880, #12910 ) ) ;
#10851 = AXIS2_PLACEMENT_3D ( 'NONE', #8988, #4310, #2004 ) ;
#10852 = VECTOR ( 'NONE', #11400, 1000.000000000000000 ) ;
#10853 = DIRECTION ( 'NONE',  ( -1.000000000000000000, -0.000000000000000000, -0.000000000000000000 ) ) ;
#10854 = CARTESIAN_POINT ( 'NONE',  ( 67.23404255319145761, 28.93147646537026318, 7.000000000000000000 ) ) ;
#10855 = CARTESIAN_POINT ( 'NONE',  ( 2.789999999999999147, -2.336989772644097574, -24.63872515616085224 ) ) ;
#10856 = EDGE_CURVE ( 'NONE', #3207, #383, #2199, .T. ) ;
#10857 = ORIENTED_EDGE ( 'NONE', *, *, #2527, .T. ) ;
#10858 = CARTESIAN_POINT ( 'NONE',  ( 0.07186813532171051899, 2.577209017047360717, -25.22589920183358814 ) ) ;
#10859 = CARTESIAN_POINT ( 'NONE',  ( 0.000000000000000000, 12.52067188844379864, -20.62201879784900882 ) ) ;
#10860 = EDGE_LOOP ( 'NONE', ( #2326, #13, #13236, #5837 ) ) ;
#10861 = DIRECTION ( 'NONE',  ( -1.000000000000000000, -0.000000000000000000, -0.000000000000000000 ) ) ;
#10862 = CARTESIAN_POINT ( 'NONE',  ( 0.000000000000000000, 0.4273491293402468805, -0.8000000000000000444 ) ) ;
#10863 = AXIS2_PLACEMENT_3D ( 'NONE', #5039, #6252, #2868 ) ;
#10864 = ORIENTED_EDGE ( 'NONE', *, *, #14729, .T. ) ;
#10865 = ORIENTED_EDGE ( 'NONE', *, *, #2481, .F. ) ;
#10866 =( LENGTH_UNIT ( ) NAMED_UNIT ( * ) SI_UNIT ( .MILLI., .METRE. ) );
#10867 = CARTESIAN_POINT ( 'NONE',  ( 1.749999999999998002, -12.52377138324206030, -25.12109765559667096 ) ) ;
#10868 = ADVANCED_FACE ( 'NONE', ( #14357 ), #8505, .T. ) ;
#10869 = ADVANCED_FACE ( 'NONE', ( #5297 ), #6430, .T. ) ;
#10870 = CARTESIAN_POINT ( 'NONE',  ( 0.7592463977762113903, 27.14986936243574078, 4.828194074574446049 ) ) ;
#10871 = LINE ( 'NONE', #14264, #14473 ) ;
#10872 = LINE ( 'NONE', #6265, #13226 ) ;
#10873 = ORIENTED_EDGE ( 'NONE', *, *, #7437, .T. ) ;
#10874 = DIRECTION ( 'NONE',  ( -1.000000000000000000, 0.000000000000000000, 0.000000000000000000 ) ) ;
#10875 = CARTESIAN_POINT ( 'NONE',  ( 0.000000000000000000, 0.000000000000000000, 0.000000000000000000 ) ) ;
#10876 = CARTESIAN_POINT ( 'NONE',  ( 1.749999999999999778, -4.458161950358378256, -17.39253030560846369 ) ) ;
#10877 = CARTESIAN_POINT ( 'NONE',  ( 4.872650870659752442, 0.4273491293402468805, -0.8000000000000000444 ) ) ;
#10878 = VERTEX_POINT ( 'NONE', #11113 ) ;
#10879 = EDGE_CURVE ( 'NONE', #7933, #7573, #13424, .T. ) ;
#10880 = ORIENTED_EDGE ( 'NONE', *, *, #9653, .F. ) ;
#10881 = EDGE_CURVE ( 'NONE', #9577, #8779, #14517, .T. ) ;
#10882 = ORIENTED_EDGE ( 'NONE', *, *, #9582, .T. ) ;
#10883 = DIRECTION ( 'NONE',  ( 1.000000000000000000, -0.000000000000000000, -0.000000000000000000 ) ) ;
#10884 = CARTESIAN_POINT ( 'NONE',  ( 0.02436607992775674525, 9.836394144776026138, -22.71065055754441531 ) ) ;
#10885 = ADVANCED_FACE ( 'NONE', ( #8815 ), #15099, .T. ) ;
#10886 = DIRECTION ( 'NONE',  ( -1.000000000000000000, -0.000000000000000000, 0.000000000000000000 ) ) ;
#10887 = CARTESIAN_POINT ( 'NONE',  ( 0.02436607992776368414, -9.836394144775550075, -22.71065055754462492 ) ) ;
#10888 = CARTESIAN_POINT ( 'NONE',  ( 80.00000000000000000, 3.469446951953614189E-15, 7.799999999999998934 ) ) ;
#10889 = CARTESIAN_POINT ( 'NONE',  ( -9.403944755730117677, -13.79473832354794816, 14.99999999999999822 ) ) ;
#10890 = ORIENTED_EDGE ( 'NONE', *, *, #11492, .T. ) ;
#10891 = DIRECTION ( 'NONE',  ( -1.000000000000000000, 0.000000000000000000, 0.000000000000000000 ) ) ;
#10892 = DIRECTION ( 'NONE',  ( -1.000000000000000000, -0.000000000000000000, -0.000000000000000000 ) ) ;
#10893 = EDGE_CURVE ( 'NONE', #4933, #6652, #728, .T. ) ;
#10894 = ORIENTED_EDGE ( 'NONE', *, *, #1571, .F. ) ;
#10895 = CARTESIAN_POINT ( 'NONE',  ( 0.000000000000000000, 0.000000000000000000, -7.800000000000010481 ) ) ;
#10896 = DIRECTION ( 'NONE',  ( -0.000000000000000000, -0.000000000000000000, 1.000000000000000000 ) ) ;
#10897 = ORIENTED_EDGE ( 'NONE', *, *, #13068, .F. ) ;
#10898 = CIRCLE ( 'NONE', #3533, 2.524999999999995914 ) ;
#10899 = VECTOR ( 'NONE', #3560, 1000.000000000000000 ) ;
#10900 = CARTESIAN_POINT ( 'NONE',  ( 0.7686372158811266564, -12.71987259277443627, 11.98841295390592876 ) ) ;
#10901 = CARTESIAN_POINT ( 'NONE',  ( 0.7686372430964724112, -17.00993931356764222, 4.022333916463534997 ) ) ;
#10902 = EDGE_LOOP ( 'NONE', ( #7979, #6898, #6093, #5360, #11845, #9900 ) ) ;
#10903 = VERTEX_POINT ( 'NONE', #11191 ) ;
#10904 = EDGE_LOOP ( 'NONE', ( #7389, #6719, #12895, #9517 ) ) ;
#10905 = CARTESIAN_POINT ( 'NONE',  ( 1.039999999999996261, -4.835383649608352208, -17.29145405592693763 ) ) ;
#10906 = B_SPLINE_CURVE_WITH_KNOTS ( 'NONE', 3,
 ( #1764, #10987, #519, #2993 ),
 .UNSPECIFIED., .F., .F.,
 ( 4, 4 ),
 ( 1.988537749986050620E-07, 0.0006916721208754055515 ),
 .UNSPECIFIED. ) ;
#10907 = CARTESIAN_POINT ( 'NONE',  ( 2.718184745196086549, -12.74223776959184207, -21.92234060054359901 ) ) ;
#10908 = DIRECTION ( 'NONE',  ( 1.000000000000000000, 0.000000000000000000, 0.000000000000000000 ) ) ;
#10909 = CARTESIAN_POINT ( 'NONE',  ( -2.321707774797442170, -4.824281976789052351, 0.000000000000000000 ) ) ;
#10910 = AXIS2_PLACEMENT_3D ( 'NONE', #11127, #7760, #12448 ) ;
#10911 = PRESENTATION_LAYER_ASSIGNMENT (  '', '', ( #7722 ) ) ;
#10913 =( GEOMETRIC_REPRESENTATION_CONTEXT ( 3 ) GLOBAL_UNCERTAINTY_ASSIGNED_CONTEXT ( ( #4478 ) ) GLOBAL_UNIT_ASSIGNED_CONTEXT ( ( #4767, #14134, #2377 ) ) REPRESENTATION_CONTEXT ( 'NONE', 'WORKASPACE' ) );
#10912 = DIRECTION ( 'NONE',  ( 1.000000000000000000, 0.000000000000000000, 2.081668171172168908E-15 ) ) ;
#10914 = EDGE_LOOP ( 'NONE', ( #2738, #8194, #13770, #4579, #1257, #12329, #5633, #7953 ) ) ;
#10915 = DIRECTION ( 'NONE',  ( 0.000000000000000000, 0.000000000000000000, 1.000000000000000000 ) ) ;
#10916 = EDGE_CURVE ( 'NONE', #14511, #7149, #14669, .T. ) ;
#10917 = VECTOR ( 'NONE', #6711, 1000.000000000000000 ) ;
#10918 = VERTEX_POINT ( 'NONE', #7441 ) ;
#10919 = ORIENTED_EDGE ( 'NONE', *, *, #10245, .F. ) ;
#10920 = DIRECTION ( 'NONE',  ( 1.000000000000000000, 0.000000000000000000, 0.000000000000000000 ) ) ;
#10921 = CARTESIAN_POINT ( 'NONE',  ( 4.000000000000000000, 4.898587196589412829E-16, 4.000000000000000000 ) ) ;
#10922 = ORIENTED_EDGE ( 'NONE', *, *, #5924, .F. ) ;
#10923 = DIRECTION ( 'NONE',  ( 1.445602896647338917E-16, -1.000000000000000000, 0.000000000000000000 ) ) ;
#10924 = AXIS2_PLACEMENT_3D ( 'NONE', #12326, #1803, #6488 ) ;
#10925 = ORIENTED_EDGE ( 'NONE', *, *, #6468, .T. ) ;
#10926 = CIRCLE ( 'NONE', #4317, 0.1000000000000011297 ) ;
#10927 = CARTESIAN_POINT ( 'NONE',  ( -5.209999999999999964, 0.000000000000000000, 0.000000000000000000 ) ) ;
#10928 = CARTESIAN_POINT ( 'NONE',  ( 0.1855656748306462045, -2.851997810081830842, 25.77772010606605235 ) ) ;
#10929 = DIRECTION ( 'NONE',  ( -1.000000000000000000, 0.000000000000000000, -0.000000000000000000 ) ) ;
#10930 = VERTEX_POINT ( 'NONE', #10887 ) ;
#10931 = FACE_OUTER_BOUND ( 'NONE', #8018, .T. ) ;
#10932 = CARTESIAN_POINT ( 'NONE',  ( 0.5279273620711159021, 12.96450951081217084, 23.73240184472501113 ) ) ;
#10933 = ORIENTED_EDGE ( 'NONE', *, *, #14182, .T. ) ;
#10934 = CARTESIAN_POINT ( 'NONE',  ( 98.48580539929344013, 0.9022481406819604643, 2.999999999999999112 ) ) ;
#10935 = AXIS2_PLACEMENT_3D ( 'NONE', #13617, #5343, #4179 ) ;
#10936 = EDGE_CURVE ( 'NONE', #10878, #5334, #6997, .T. ) ;
#10937 = CARTESIAN_POINT ( 'NONE',  ( 0.000000000000000000, 18.28042085475278000, 15.74360496233386719 ) ) ;
#10938 = ORIENTED_EDGE ( 'NONE', *, *, #685, .F. ) ;
#10939 = EDGE_LOOP ( 'NONE', ( #3882, #10136, #12304, #1604 ) ) ;
#10940 = PLANE ( 'NONE',  #8534 ) ;
#10941 = CYLINDRICAL_SURFACE ( 'NONE', #8305, 8.400000000000000355 ) ;
#10942 = ADVANCED_FACE ( 'NONE', ( #13506 ), #10051, .T. ) ;
#10943 = FACE_BOUND ( 'NONE', #7624, .T. ) ;
#10944 = VECTOR ( 'NONE', #2706, 1000.000000000000000 ) ;
#10945 = CARTESIAN_POINT ( 'NONE',  ( 2.789999999999999147, 18.28042085475301093, -15.74360496233361673 ) ) ;
#10946 = AXIS2_PLACEMENT_3D ( 'NONE', #680, #4376, #982 ) ;
#10947 = ORIENTED_EDGE ( 'NONE', *, *, #14886, .T. ) ;
#10948 = DIRECTION ( 'NONE',  ( -1.000000000000000000, -0.000000000000000000, -0.000000000000000000 ) ) ;
#10949 = CARTESIAN_POINT ( 'NONE',  ( 0.000000000000000000, 0.000000000000000000, 7.000000000000000000 ) ) ;
#10950 =( GEOMETRIC_REPRESENTATION_CONTEXT ( 3 ) GLOBAL_UNCERTAINTY_ASSIGNED_CONTEXT ( ( #13304 ) ) GLOBAL_UNIT_ASSIGNED_CONTEXT ( ( #8541, #5020, #14390 ) ) REPRESENTATION_CONTEXT ( 'NONE', 'WORKASPACE' ) );
#10951 = DIRECTION ( 'NONE',  ( -1.000000000000000000, 0.000000000000000000, 0.000000000000000000 ) ) ;
#10952 = ADVANCED_FACE ( 'NONE', ( #7663 ), #14442, .T. ) ;
#10953 = EDGE_CURVE ( 'NONE', #883, #13784, #6744, .T. ) ;
#10954 = VERTEX_POINT ( 'NONE', #14746 ) ;
#10955 = ORIENTED_EDGE ( 'NONE', *, *, #13199, .T. ) ;
#10956 = CIRCLE ( 'NONE', #6796, 14.01039946648074341 ) ;
#10957 = CIRCLE ( 'NONE', #14157, 24.12539914357697768 ) ;
#10958 = ORIENTED_EDGE ( 'NONE', *, *, #2721, .F. ) ;
#10959 = CARTESIAN_POINT ( 'NONE',  ( 0.000000000000000000, 0.000000000000000000, 0.000000000000000000 ) ) ;
#10960 = CARTESIAN_POINT ( 'NONE',  ( 2.764680872513208154, 9.232963481057765875, 11.36963888406690870 ) ) ;
#10961 = AXIS2_PLACEMENT_3D ( 'NONE', #8830, #14532, #14377 ) ;
#10962 = CARTESIAN_POINT ( 'NONE',  ( 0.000000000000000000, 0.000000000000000000, -10.00000000000000000 ) ) ;
#10963 = DIRECTION ( 'NONE',  ( -1.000000000000000000, 0.000000000000000000, 0.000000000000000000 ) ) ;
#10964 = DIRECTION ( 'NONE',  ( 0.000000000000000000, 0.000000000000000000, 1.000000000000000000 ) ) ;
#10965 = CIRCLE ( 'NONE', #10241, 3.000000000000000888 ) ;
#10966 = DIRECTION ( 'NONE',  ( -0.1643989873053572359, 0.9863939238321437486, 0.000000000000000000 ) ) ;
#10967 = ORIENTED_EDGE ( 'NONE', *, *, #2679, .T. ) ;
#10968 = CARTESIAN_POINT ( 'NONE',  ( -16.02604379927987566, -7.138402084508245871, -5.000000000000000000 ) ) ;
#10969 = CARTESIAN_POINT ( 'NONE',  ( 13.28797974610714761, -21.11867004231547540, -130.1575142076926852 ) ) ;
#10970 = ADVANCED_FACE ( 'NONE', ( #1677 ), #9693, .T. ) ;
#10971 = VERTEX_POINT ( 'NONE', #4213 ) ;
#10972 = DIRECTION ( 'NONE',  ( 1.000000000000000000, 0.000000000000000000, 0.000000000000000000 ) ) ;
#10973 = CARTESIAN_POINT ( 'NONE',  ( 93.49175023922396122, 0.6585002008270834928, 4.000000000000000000 ) ) ;
#10974 = CARTESIAN_POINT ( 'NONE',  ( 79.18363542992865689, -10.13606076167855541, 3.000000000000002665 ) ) ;
#10975 = EDGE_CURVE ( 'NONE', #1423, #13868, #8231, .T. ) ;
#10976 = ORIENTED_EDGE ( 'NONE', *, *, #2950, .T. ) ;
#10977 = VECTOR ( 'NONE', #5614, 1000.000000000000000 ) ;
#10978 = CIRCLE ( 'NONE', #10739, 3.799999999999998934 ) ;
#10979 = CARTESIAN_POINT ( 'NONE',  ( 2.021362784118869715, -11.98841295390606554, 12.71987259277430837 ) ) ;
#10981 = VECTOR ( 'NONE', #11584, 1000.000000000000000 ) ;
#10980 = DIRECTION ( 'NONE',  ( -1.000000000000000000, -0.000000000000000000, -0.000000000000000000 ) ) ;
#10982 = ORIENTED_EDGE ( 'NONE', *, *, #2163, .F. ) ;
#10983 = VECTOR ( 'NONE', #1970, 1000.000000000000000 ) ;
#10984 = EDGE_LOOP ( 'NONE', ( #5008, #10160, #5000, #5776 ) ) ;
#10985 = VERTEX_POINT ( 'NONE', #7596 ) ;
#10986 = CARTESIAN_POINT ( 'NONE',  ( 2.765633920072235075, 24.63872515616082737, -2.336989772644355590 ) ) ;
#10987 = CARTESIAN_POINT ( 'NONE',  ( 2.782672486186223093, 5.204526028255688885, 13.44898112152240266 ) ) ;
#10988 = EDGE_CURVE ( 'NONE', #4472, #8917, #13269, .T. ) ;
#10989 = DIRECTION ( 'NONE',  ( 1.000000000000000000, -0.000000000000000000, -0.000000000000000000 ) ) ;
#10990 = CARTESIAN_POINT ( 'NONE',  ( 1.039999999999996927, 20.02152543075374069, -19.67366047555508501 ) ) ;
#10991 = CARTESIAN_POINT ( 'NONE',  ( 0.000000000000000000, 3.361026734705063745E-15, 7.799999999999990052 ) ) ;
#10992 = B_SPLINE_CURVE_WITH_KNOTS ( 'NONE', 3,
 ( #6496, #11180, #7726, #11483, #9112, #8801 ),
 .UNSPECIFIED., .F., .F.,
 ( 4, 2, 4 ),
 ( 4.462636882221166670E-07, 0.001879885203074807814, 0.003759324142461393462 ),
 .UNSPECIFIED. ) ;
#10993 = AXIS2_PLACEMENT_3D ( 'NONE', #2471, #1302, #3843 ) ;
#10994 = DIRECTION ( 'NONE',  ( 0.000000000000000000, 0.000000000000000000, 1.000000000000000000 ) ) ;
#10995 = ORIENTED_EDGE ( 'NONE', *, *, #5658, .F. ) ;
#10996 = CARTESIAN_POINT ( 'NONE',  ( 2.789999999999999147, -11.04103753892265694, -8.624777288397918795 ) ) ;
#10997 = VECTOR ( 'NONE', #10162, 1000.000000000000000 ) ;
#10998 = CIRCLE ( 'NONE', #12477, 3.799999999999999378 ) ;
#10999 = ORIENTED_EDGE ( 'NONE', *, *, #13052, .T. ) ;
#11000 = VERTEX_POINT ( 'NONE', #12108 ) ;
#11001 = DIRECTION ( 'NONE',  ( -1.000000000000000000, 0.000000000000000000, 0.000000000000000000 ) ) ;
#11002 = FILL_AREA_STYLE ('',( #3096 ) ) ;
#11003 = EDGE_CURVE ( 'NONE', #188, #5333, #3797, .T. ) ;
#11004 = VERTEX_POINT ( 'NONE', #969 ) ;
#11005 = VECTOR ( 'NONE', #9405, 1000.000000000000000 ) ;
#11006 = AXIS2_PLACEMENT_3D ( 'NONE', #2579, #335, #3805 ) ;
#11007 = UNCERTAINTY_MEASURE_WITH_UNIT (LENGTH_MEASURE( 1.000000000000000082E-05 ), #253, 'distance_accuracy_value', 'NONE');
#11008 = CARTESIAN_POINT ( 'NONE',  ( 72.68384697807672978, 11.35494834827056110, 2.999999999999999112 ) ) ;
#11009 = EDGE_LOOP ( 'NONE', ( #3226, #6722, #6394, #14241 ) ) ;
#11010 = B_SPLINE_CURVE_WITH_KNOTS ( 'NONE', 3,
 ( #5158, #8591, #1451, #10821 ),
 .UNSPECIFIED., .F., .F.,
 ( 4, 4 ),
 ( 2.451234579287542699E-07, 0.0006917187676826499999 ),
 .UNSPECIFIED. ) ;
#11011 = CARTESIAN_POINT ( 'NONE',  ( 0.1882238946918237121, 25.78859396478527799, -2.857713464478781162 ) ) ;
#11012 = DIRECTION ( 'NONE',  ( -5.480158469902919838E-17, -1.051478716308701618E-16, -1.000000000000000000 ) ) ;
#11013 = LINE ( 'NONE', #8627, #845 ) ;
#11014 = AXIS2_PLACEMENT_3D ( 'NONE', #8105, #4727, #2189 ) ;
#11015 = VECTOR ( 'NONE', #3654, 1000.000000000000000 ) ;
#11016 = DIRECTION ( 'NONE',  ( 0.9863939238321436376, 0.1643989873053573192, 0.000000000000000000 ) ) ;
#11017 = ADVANCED_FACE ( 'NONE', ( #6736 ), #13737, .T. ) ;
#11018 = CARTESIAN_POINT ( 'NONE',  ( 64.81187243050929681, 34.42083816749791936, 5.000000000000000888 ) ) ;
#11019 = ORIENTED_EDGE ( 'NONE', *, *, #13983, .F. ) ;
#11020 = CARTESIAN_POINT ( 'NONE',  ( 0.000000000000000000, 12.52067188844351442, 20.62201879784919001 ) ) ;
#11021 = CARTESIAN_POINT ( 'NONE',  ( 0.02436607992776064838, 18.55949924794892780, 16.37294372382865504 ) ) ;
#11022 = ORIENTED_EDGE ( 'NONE', *, *, #14334, .F. ) ;
#11023 = ORIENTED_EDGE ( 'NONE', *, *, #14214, .T. ) ;
#11024 = DIRECTION ( 'NONE',  ( -0.000000000000000000, -0.000000000000000000, -1.000000000000000000 ) ) ;
#11025 = CARTESIAN_POINT ( 'NONE',  ( 2.031033491000346913, -12.05173163741705444, -24.80232951178391332 ) ) ;
#11026 = DIRECTION ( 'NONE',  ( -1.000000000000000000, -0.000000000000000000, -0.000000000000000000 ) ) ;
#11027 = AXIS2_PLACEMENT_3D ( 'NONE', #2071, #7687, #5692 ) ;
#11028 = EDGE_CURVE ( 'NONE', #7572, #5935, #8971, .T. ) ;
#11029 = CARTESIAN_POINT ( 'NONE',  ( 1.394999999999999574, -27.68468304288262161, 4.633866840648820151 ) ) ;
#11030 = EDGE_CURVE ( 'NONE', #12114, #8358, #8694, .T. ) ;
#11031 = ORIENTED_EDGE ( 'NONE', *, *, #10936, .F. ) ;
#11032 = PLANE ( 'NONE',  #3891 ) ;
#11033 = DIRECTION ( 'NONE',  ( 1.000000000000000000, 0.000000000000000000, 0.000000000000000000 ) ) ;
#11034 = CARTESIAN_POINT ( 'NONE',  ( 1.394999999999999574, -12.96210679857803960, 24.89775460606827551 ) ) ;
#11035 = CARTESIAN_POINT ( 'NONE',  ( 19.25177984293773648, 7.759396820770405157, 4.000000000000003553 ) ) ;
#11036 = ORIENTED_EDGE ( 'NONE', *, *, #6185, .T. ) ;
#11037 = AXIS2_PLACEMENT_3D ( 'NONE', #8657, #4059, #13346 ) ;
#11038 = ORIENTED_EDGE ( 'NONE', *, *, #5699, .F. ) ;
#11039 = ORIENTED_EDGE ( 'NONE', *, *, #9111, .F. ) ;
#11040 = CARTESIAN_POINT ( 'NONE',  ( 67.23404255319145761, 28.93147646537026318, 3.000000000000002665 ) ) ;
#11041 = DIRECTION ( 'NONE',  ( 0.000000000000000000, 0.8660254037844433705, -0.4999999999999918954 ) ) ;
#11042 = CARTESIAN_POINT ( 'NONE',  ( 2.321707774797442170, -4.824281976789052351, -0.8000000000000000444 ) ) ;
#11043 = CARTESIAN_POINT ( 'NONE',  ( 2.257825459230522913, -4.993157874727630841, -26.58873630738057159 ) ) ;
#11044 = SHAPE_DEFINITION_REPRESENTATION ( #610, #7313 ) ;
#11045 = CARTESIAN_POINT ( 'NONE',  ( 0.000000000000000000, 0.000000000000000000, -0.8000000000000000444 ) ) ;
#11046 = PRODUCT ( 'circlip for shafts normal_din_Circlip DIN 471 - 8 x 0.8', 'circlip for shafts normal_din_Circlip DIN 471 - 8 x 0.8', '', ( #6361 ) ) ;
#11047 = EDGE_CURVE ( 'NONE', #3303, #13854, #11708, .T. ) ;
#11048 = CARTESIAN_POINT ( 'NONE',  ( 86.00000000000000000, 7.347880794884121708E-16, 5.500000000000000000 ) ) ;
#11049 = CARTESIAN_POINT ( 'NONE',  ( 2.604434283110813819, 12.84444904262057818, -22.53097606932971075 ) ) ;
#11050 = VECTOR ( 'NONE', #9200, 1000.000000000000000 ) ;
#11051 = ORIENTED_EDGE ( 'NONE', *, *, #3467, .F. ) ;
#11052 = DIRECTION ( 'NONE',  ( -0.000000000000000000, -0.000000000000000000, -1.000000000000000000 ) ) ;
#11053 = CARTESIAN_POINT ( 'NONE',  ( 2.765633920072235519, 24.15498966839970052, -5.391175441198366336 ) ) ;
#11054 = CARTESIAN_POINT ( 'NONE',  ( 1.039999999999999369, 12.55714665599987079, 12.83329210556836308 ) ) ;
#11055 = ORIENTED_EDGE ( 'NONE', *, *, #4883, .F. ) ;
#11056 = EDGE_CURVE ( 'NONE', #4228, #9067, #3214, .T. ) ;
#11057 = DIRECTION ( 'NONE',  ( -1.000000000000000000, -0.000000000000000000, -0.000000000000000000 ) ) ;
#11058 = DIRECTION ( 'NONE',  ( 0.000000000000000000, 0.000000000000000000, 1.000000000000000000 ) ) ;
#11059 = ORIENTED_EDGE ( 'NONE', *, *, #3847, .T. ) ;
#11060 = VERTEX_POINT ( 'NONE', #7897 ) ;
#11061 = DIRECTION ( 'NONE',  ( -0.000000000000000000, -0.000000000000000000, -1.000000000000000000 ) ) ;
#11062 = DIRECTION ( 'NONE',  ( -0.000000000000000000, -0.000000000000000000, 1.000000000000000000 ) ) ;
#11063 = CARTESIAN_POINT ( 'NONE',  ( 0.7795480803411072301, -16.99607982911238935, -4.029281904976810935 ) ) ;
#11064 = FACE_OUTER_BOUND ( 'NONE', #14595, .T. ) ;
#11065 = DIRECTION ( 'NONE',  ( -1.000000000000000000, -0.000000000000000000, -0.000000000000000000 ) ) ;
#11066 = ADVANCED_FACE ( 'NONE', ( #8118 ), #15121, .T. ) ;
#11067 = EDGE_CURVE ( 'NONE', #13334, #15084, #1844, .T. ) ;
#11068 = CARTESIAN_POINT ( 'NONE',  ( 2.337784053193427081, 11.13074453164202993, 12.42068120944084697 ) ) ;
#11069 = ORIENTED_EDGE ( 'NONE', *, *, #3847, .F. ) ;
#11070 = PLANE ( 'NONE',  #3849 ) ;
#11071 = DIRECTION ( 'NONE',  ( 1.000000000000000000, 1.445602896647338917E-16, -0.000000000000000000 ) ) ;
#11072 = FILL_AREA_STYLE_COLOUR ( '', #12176 ) ;
#11073 = VERTEX_POINT ( 'NONE', #12573 ) ;
#11074 = ORIENTED_EDGE ( 'NONE', *, *, #8609, .F. ) ;
#11075 = VERTEX_POINT ( 'NONE', #10119 ) ;
#11076 = EDGE_CURVE ( 'NONE', #12714, #4008, #4305, .T. ) ;
#11077 = CARTESIAN_POINT ( 'NONE',  ( 2.764680872515351329, -11.36963888406680923, -9.232963481057881339 ) ) ;
#11078 = EDGE_CURVE ( 'NONE', #9761, #2630, #13652, .T. ) ;
#11079 = SURFACE_SIDE_STYLE ('',( #8683 ) ) ;
#11080 = ORIENTED_EDGE ( 'NONE', *, *, #7905, .T. ) ;
#11081 = EDGE_CURVE ( 'NONE', #12694, #1885, #8219, .T. ) ;
#11082 = FACE_OUTER_BOUND ( 'NONE', #8155, .T. ) ;
#11083 = VERTEX_POINT ( 'NONE', #4362 ) ;
#11084 = DIRECTION ( 'NONE',  ( 0.000000000000000000, 0.000000000000000000, 1.000000000000000000 ) ) ;
#11085 = DIRECTION ( 'NONE',  ( -0.000000000000000000, -0.000000000000000000, -1.000000000000000000 ) ) ;
#11086 = ADVANCED_FACE ( 'NONE', ( #12719 ), #3429, .F. ) ;
#11087 = CARTESIAN_POINT ( 'NONE',  ( 0.02436607992775717893, -9.836394144775869819, 22.71065055754449347 ) ) ;
#11088 = B_SPLINE_CURVE_WITH_KNOTS ( 'NONE', 3,
 ( #4125, #10107, #7654, #801 ),
 .UNSPECIFIED., .F., .F.,
 ( 4, 4 ),
 ( 2.324263106244698315E-07, 0.0006888201370294716810 ),
 .UNSPECIFIED. ) ;
#11089 = FACE_OUTER_BOUND ( 'NONE', #1795, .T. ) ;
#11090 = CARTESIAN_POINT ( 'NONE',  ( 0.07186814640506923590, 12.74240566898984284, 21.92302674874967749 ) ) ;
#11091 = ORIENTED_EDGE ( 'NONE', *, *, #12490, .T. ) ;
#11092 = DIRECTION ( 'NONE',  ( 1.000000000000000000, 0.000000000000000000, 0.000000000000000000 ) ) ;
#11093 = CARTESIAN_POINT ( 'NONE',  ( 0.000000000000000000, 13.87420763704361448, -1.948757464274226470 ) ) ;
#11094 = ORIENTED_EDGE ( 'NONE', *, *, #13137, .T. ) ;
#11095 = ORIENTED_EDGE ( 'NONE', *, *, #13073, .F. ) ;
#11096 = DIRECTION ( 'NONE',  ( -0.000000000000000000, -0.000000000000000000, -1.000000000000000000 ) ) ;
#11097 = FACE_BOUND ( 'NONE', #9215, .T. ) ;
#11098 = FACE_OUTER_BOUND ( 'NONE', #4107, .T. ) ;
#11099 = DIRECTION ( 'NONE',  ( 1.000000000000000000, 0.000000000000000000, 0.000000000000000000 ) ) ;
#11100 = VERTEX_POINT ( 'NONE', #6888 ) ;
#11101 = CYLINDRICAL_SURFACE ( 'NONE', #8547, 13.19999999999999929 ) ;
#11102 = CARTESIAN_POINT ( 'NONE',  ( 1.039999999999997593, -12.52377138324241557, 25.12109765559648977 ) ) ;
#11103 = LINE ( 'NONE', #1435, #4408 ) ;
#11104 =( NAMED_UNIT ( * ) PLANE_ANGLE_UNIT ( ) SI_UNIT ( $, .RADIAN. ) );
#11105 = AXIS2_PLACEMENT_3D ( 'NONE', #3405, #11611, #5791 ) ;
#11106 = EDGE_LOOP ( 'NONE', ( #3367, #13695, #319, #6471 ) ) ;
#11107 = ORIENTED_EDGE ( 'NONE', *, *, #13622, .T. ) ;
#11108 = EDGE_LOOP ( 'NONE', ( #8995, #12957, #14798, #9171, #12678, #8145 ) ) ;
#11109 = CARTESIAN_POINT ( 'NONE',  ( 1.039999999999996483, -27.76164181293054511, 4.147968289691193355 ) ) ;
#11110 = CYLINDRICAL_SURFACE ( 'NONE', #9279, 13.19999999999999929 ) ;
#11111 = EDGE_CURVE ( 'NONE', #8828, #9867, #4759, .T. ) ;
#11112 = CARTESIAN_POINT ( 'NONE',  ( 1.749999999999998002, -25.12109765559643648, -12.52377138324252570 ) ) ;
#11113 = CARTESIAN_POINT ( 'NONE',  ( -19.40394475573012301, -13.79473832354794993, 16.99999999999999645 ) ) ;
#11114 = CARTESIAN_POINT ( 'NONE',  ( 2.790000000000077751, 24.22524813288762147, 2.133839912090885527 ) ) ;
#11115 = CARTESIAN_POINT ( 'NONE',  ( 1.749999999999998002, 27.76164181293051669, 4.147968289691386090 ) ) ;
#11116 = DIRECTION ( 'NONE',  ( 0.000000000000000000, 0.000000000000000000, 1.000000000000000000 ) ) ;
#11117 = ORIENTED_EDGE ( 'NONE', *, *, #1816, .F. ) ;
#11118 = CARTESIAN_POINT ( 'NONE',  ( 0.02436607992776325046, 16.37294372382858398, 18.55949924794898465 ) ) ;
#11119 = DIRECTION ( 'NONE',  ( 0.000000000000000000, 0.000000000000000000, -1.000000000000000000 ) ) ;
#11120 = VERTEX_POINT ( 'NONE', #7963 ) ;
#11121 = CARTESIAN_POINT ( 'NONE',  ( 0.1374368770859596967, -4.808326913195983821, -0.8000000000000000444 ) ) ;
#11122 = LINE ( 'NONE', #445, #4327 ) ;
#11123 = ORIENTED_EDGE ( 'NONE', *, *, #14249, .F. ) ;
#11124 = VERTEX_POINT ( 'NONE', #13804 ) ;
#11125 = CARTESIAN_POINT ( 'NONE',  ( 2.789999999999999147, 7.739906618939895289, -10.88091150984218380 ) ) ;
#11126 = CARTESIAN_POINT ( 'NONE',  ( 0.02436607992776455150, 5.391175441198956086, -24.15498966839956907 ) ) ;
#11127 = CARTESIAN_POINT ( 'NONE',  ( -19.40394475573012301, -7.794738323547950820, 16.99999999999999645 ) ) ;
#11128 = DIRECTION ( 'NONE',  ( 0.000000000000000000, 0.000000000000000000, 1.000000000000000000 ) ) ;
#11129 = AXIS2_PLACEMENT_3D ( 'NONE', #5854, #12600, #2079 ) ;
#11130 = EDGE_CURVE ( 'NONE', #11997, #9762, #12509, .T. ) ;
#11131 = CLOSED_SHELL ( 'NONE', ( #15026, #8484, #727, #7173, #13235, #6920, #4146, #10298, #12620, #10322, #8806, #8272, #13100, #14633, #12935, #8856, #9853, #7095, #11017, #5978, #15222, #9015, #9749, #716, #5715, #3990, #2499 ) ) ;
#11132 = CARTESIAN_POINT ( 'NONE',  ( 2.604434404052930141, 19.17825124759803401, -17.45907811351434802 ) ) ;
#11133 = VERTEX_POINT ( 'NONE', #9049 ) ;
#11134 = DIRECTION ( 'NONE',  ( -1.000000000000000000, -0.000000000000000000, -0.000000000000000000 ) ) ;
#11135 = CIRCLE ( 'NONE', #5752, 0.7500000000000002220 ) ;
#11136 = AXIS2_PLACEMENT_3D ( 'NONE', #9998, #14700, #10790 ) ;
#11137 = CARTESIAN_POINT ( 'NONE',  ( 98.33955663538051795, 3.898681236723621879, 6.000000000000000000 ) ) ;
#11138 = AXIS2_PLACEMENT_3D ( 'NONE', #8171, #4285, #12843 ) ;
#11139 = PRODUCT_DEFINITION ( 'UNKNOWN', '', #12636, #542 ) ;
#11140 = EDGE_CURVE ( 'NONE', #3735, #14731, #4551, .T. ) ;
#11141 = EDGE_CURVE ( 'NONE', #2895, #5216, #11886, .T. ) ;
#11142 = ORIENTED_EDGE ( 'NONE', *, *, #6450, .F. ) ;
#11143 = VERTEX_POINT ( 'NONE', #3573 ) ;
#11144 = EDGE_LOOP ( 'NONE', ( #6610, #6806, #8179, #5777 ) ) ;
#11145 = CARTESIAN_POINT ( 'NONE',  ( 2.782672435525938681, -11.23174270417322695, -9.044896821682320009 ) ) ;
#11146 = AXIS2_PLACEMENT_3D ( 'NONE', #10069, #2843, #8752 ) ;
#11147 = CARTESIAN_POINT ( 'NONE',  ( 2.789999999999999147, -20.62201879784904079, -12.52067188844374179 ) ) ;
#11148 = CIRCLE ( 'NONE', #9439, 4.000000000000000000 ) ;
#11149 = AXIS2_PLACEMENT_3D ( 'NONE', #14594, #4066, #588 ) ;
#11150 = UNCERTAINTY_MEASURE_WITH_UNIT (LENGTH_MEASURE( 1.000000000000000082E-05 ), #15070, 'distance_accuracy_value', 'NONE');
#11151 = DIRECTION ( 'NONE',  ( -1.000000000000000000, -0.000000000000000000, -0.000000000000000000 ) ) ;
#11152 = CARTESIAN_POINT ( 'NONE',  ( 0.5321745227542252765, -19.66801664102716884, 18.57583492944412384 ) ) ;
#11153 = EDGE_LOOP ( 'NONE', ( #7074, #9879, #8170, #13432, #802, #1173, #1276, #2219 ) ) ;
#11154 = CARTESIAN_POINT ( 'NONE',  ( 59.05334708265790056, 38.04890259842303379, 6.000000000000000000 ) ) ;
#11155 = DIRECTION ( 'NONE',  ( 0.000000000000000000, 0.000000000000000000, 1.000000000000000000 ) ) ;
#11156 = ADVANCED_FACE ( 'NONE', ( #5959 ), #3312, .T. ) ;
#11157 = VECTOR ( 'NONE', #9968, 1000.000000000000000 ) ;
#11158 = EDGE_CURVE ( 'NONE', #7278, #12816, #10667, .T. ) ;
#11159 = DIRECTION ( 'NONE',  ( 0.000000000000000000, 0.000000000000000000, 1.000000000000000000 ) ) ;
#11160 = AXIS2_PLACEMENT_3D ( 'NONE', #3256, #3409, #6941 ) ;
#11161 = FACE_OUTER_BOUND ( 'NONE', #5412, .T. ) ;
#11162 = ADVANCED_FACE ( 'NONE', ( #9346 ), #12941, .T. ) ;
#11163 = CYLINDRICAL_SURFACE ( 'NONE', #2629, 13.20000000000000284 ) ;
#11164 = VERTEX_POINT ( 'NONE', #9641 ) ;
#11165 = DIRECTION ( 'NONE',  ( 0.000000000000000000, 0.000000000000000000, 1.000000000000000000 ) ) ;
#11166 = PRODUCT ( 'short pitch roller chain wheel_s_iso_Chain wheel ISO - 20Z 05B-1 --20SA8.0N', 'short pitch roller chain wheel_s_iso_Chain wheel ISO - 20Z 05B-1 --20SA8.0N', '', ( #11192 ) ) ;
#11167 = CARTESIAN_POINT ( 'NONE',  ( 0.7592463977762105021, -27.14986936243570526, -4.828194074574642336 ) ) ;
#11168 = ORIENTED_EDGE ( 'NONE', *, *, #13422, .F. ) ;
#11169 = ORIENTED_EDGE ( 'NONE', *, *, #5143, .T. ) ;
#11170 = CARTESIAN_POINT ( 'NONE',  ( -6.210711756101269051E-14, 5.211197193340876943, -13.21862218141511036 ) ) ;
#11172 = DIRECTION ( 'NONE',  ( 0.000000000000000000, 0.000000000000000000, -1.000000000000000000 ) ) ;
#11171 = AXIS2_PLACEMENT_3D ( 'NONE', #1731, #11026, #6188 ) ;
#11173 = EDGE_CURVE ( 'NONE', #11143, #4786, #10576, .T. ) ;
#11174 = AXIS2_PLACEMENT_3D ( 'NONE', #2633, #151, #5023 ) ;
#11175 = CIRCLE ( 'NONE', #11160, 2.999999999999988898 ) ;
#11176 = SHAPE_REPRESENTATION_RELATIONSHIP ( 'NONE' , 'NONE' ,  #2588, #15172 ) ;
#11177 = CARTESIAN_POINT ( 'NONE',  ( 1.749999999999998002, 4.147968289691286614, 27.76164181293053090 ) ) ;
#11178 = CARTESIAN_POINT ( 'NONE',  ( 2.789999999999999147, -8.624777288397876163, 11.04103753892268713 ) ) ;
#11179 = ORIENTED_EDGE ( 'NONE', *, *, #3036, .F. ) ;
#11180 = CARTESIAN_POINT ( 'NONE',  ( 2.030753616560877717, 12.05220173035473863, -24.80264696524870516 ) ) ;
#11181 = DIRECTION ( 'NONE',  ( 0.000000000000000000, 1.000000000000000000, 1.099230717450651647E-14 ) ) ;
#11182 = ORIENTED_EDGE ( 'NONE', *, *, #9106, .T. ) ;
#11183 = CIRCLE ( 'NONE', #1128, 14.01039946648074341 ) ;
#11184 = CARTESIAN_POINT ( 'NONE',  ( 2.030753605846573162, -27.31305418910207905, -3.797885586973501759 ) ) ;
#11185 = ORIENTED_EDGE ( 'NONE', *, *, #2329, .T. ) ;
#11186 = ORIENTED_EDGE ( 'NONE', *, *, #7737, .F. ) ;
#11187 = CARTESIAN_POINT ( 'NONE',  ( 0.7592463896980118365, -19.12676442129330212, -19.86438386685682644 ) ) ;
#11188 = CARTESIAN_POINT ( 'NONE',  ( -20.63749999999999929, 5.633375276077824112E-16, 4.599999999999999645 ) ) ;
#11189 = AXIS2_PLACEMENT_3D ( 'NONE', #10602, #7215, #10451 ) ;
#11190 = CARTESIAN_POINT ( 'NONE',  ( 14.40394475573011945, -10.79473832354794460, 6.000000000000000000 ) ) ;
#11191 = CARTESIAN_POINT ( 'NONE',  ( 2.789999999999999147, -5.535312321042557215, -23.48180575137735815 ) ) ;
#11192 = PRODUCT_CONTEXT ( 'NONE', #13103, 'mechanical' ) ;
#11193 = CARTESIAN_POINT ( 'NONE',  ( 2.765633920072239516, -2.336989772644097574, -24.63872515616085224 ) ) ;
#11194 = MECHANICAL_DESIGN_GEOMETRIC_PRESENTATION_REPRESENTATION (  '', ( #641 ), #10469 ) ;
#11195 = DIRECTION ( 'NONE',  ( 0.000000000000000000, -0.000000000000000000, 1.000000000000000000 ) ) ;
#11196 = DIRECTION ( 'NONE',  ( -1.000000000000000000, -0.000000000000000000, 0.000000000000000000 ) ) ;
#11197 = ORIENTED_EDGE ( 'NONE', *, *, #7945, .F. ) ;
#11198 = CYLINDRICAL_SURFACE ( 'NONE', #11735, 5.000000000000000888 ) ;
#11199 = B_SPLINE_CURVE_WITH_KNOTS ( 'NONE', 3,
 ( #10807, #2581, #12262, #262, #4977, #13331, #13261, #10876 ),
 .UNSPECIFIED., .F., .F.,
 ( 4, 2, 2, 4 ),
 ( 2.154797737796021283E-07, 0.001895231411415137677, 0.002842739377235819348, 0.003790247343056500368 ),
 .UNSPECIFIED. ) ;
#11200 = DIRECTION ( 'NONE',  ( 0.000000000000000000, 0.000000000000000000, 1.000000000000000000 ) ) ;
#11201 = CARTESIAN_POINT ( 'NONE',  ( 2.771810350101906906, 13.58893811801144658, -5.219853812240780044 ) ) ;
#11202 = VECTOR ( 'NONE', #7320, 1000.000000000000000 ) ;
#11203 = VERTEX_POINT ( 'NONE', #26 ) ;
#11204 = AXIS2_PLACEMENT_3D ( 'NONE', #1725, #6408, #11092 ) ;
#11205 = EDGE_CURVE ( 'NONE', #3461, #6683, #6502, .T. ) ;
#11206 = CYLINDRICAL_SURFACE ( 'NONE', #10466, 4.999999999999997335 ) ;
#11207 = CARTESIAN_POINT ( 'NONE',  ( -20.63749999999999574, 0.000000000000000000, 0.000000000000000000 ) ) ;
#11208 = ORIENTED_EDGE ( 'NONE', *, *, #3539, .T. ) ;
#11209 = AXIS2_PLACEMENT_3D ( 'NONE', #11758, #9375, #12980 ) ;
#11210 = CIRCLE ( 'NONE', #13165, 24.12539914357697413 ) ;
#11211 = ORIENTED_EDGE ( 'NONE', *, *, #7614, .T. ) ;
#11212 = SURFACE_STYLE_USAGE ( .BOTH. , #13524 ) ;
#11213 = CARTESIAN_POINT ( 'NONE',  ( 2.789999999999999147, -14.19996452731192527, 4.595504208219980846 ) ) ;
#11214 = CARTESIAN_POINT ( 'NONE',  ( 65.94650549498811642, -33.90026220706953808, 4.000000000000000000 ) ) ;
#11215 = CARTESIAN_POINT ( 'NONE',  ( 0.07181525068722535710, -2.576941577947229334, -25.22524549359953383 ) ) ;
#11216 = DIRECTION ( 'NONE',  ( -1.000000000000000000, -0.000000000000000000, -0.000000000000000000 ) ) ;
#11217 = CARTESIAN_POINT ( 'NONE',  ( 0.02436607992776455150, -22.71065055754459650, 9.836394144775621129 ) ) ;
#11218 = DIRECTION ( 'NONE',  ( -0.000000000000000000, -0.000000000000000000, 1.000000000000000000 ) ) ;
#11219 = ADVANCED_FACE ( 'NONE', ( #14029 ), #10505, .F. ) ;
#11220 = ORIENTED_EDGE ( 'NONE', *, *, #10084, .T. ) ;
#11221 = CARTESIAN_POINT ( 'NONE',  ( 0.000000000000000000, 5.535312321042724193, 23.48180575137730841 ) ) ;
#11222 = AXIS2_PLACEMENT_3D ( 'NONE', #14513, #7515, #6356 ) ;
#11223 = B_SPLINE_CURVE_WITH_KNOTS ( 'NONE', 3,
 ( #14178, #4582, #14252, #1260 ),
 .UNSPECIFIED., .F., .F.,
 ( 4, 4 ),
 ( 1.988537749986050620E-07, 0.0006916721208754038168 ),
 .UNSPECIFIED. ) ;
#11224 = LINE ( 'NONE', #9912, #7962 ) ;
#11225 = EDGE_CURVE ( 'NONE', #13039, #9942, #7497, .T. ) ;
#11226 = EDGE_LOOP ( 'NONE', ( #5088, #8252, #14645, #7304 ) ) ;
#11227 = EDGE_CURVE ( 'NONE', #9211, #7272, #3496, .T. ) ;
#11228 = ORIENTED_EDGE ( 'NONE', *, *, #13312, .F. ) ;
#11229 = ORIENTED_EDGE ( 'NONE', *, *, #5864, .T. ) ;
#11230 = EDGE_LOOP ( 'NONE', ( #5428, #9732, #12842, #5054 ) ) ;
#11231 = CARTESIAN_POINT ( 'NONE',  ( 0.02531912748464804769, 9.232963481057765875, 11.36963888406690870 ) ) ;
#11232 =( LENGTH_UNIT ( ) NAMED_UNIT ( * ) SI_UNIT ( .MILLI., .METRE. ) );
#11233 = AXIS2_PLACEMENT_3D ( 'NONE', #3425, #178, #4670 ) ;
#11234 = AXIS2_PLACEMENT_3D ( 'NONE', #941, #3598, #5645 ) ;
#11235 = CARTESIAN_POINT ( 'NONE',  ( 2.789999999999999147, 9.232963481057765875, 11.36963888406690870 ) ) ;
#11236 = DIRECTION ( 'NONE',  ( -1.000000000000000000, -0.000000000000000000, -0.000000000000000000 ) ) ;
#11237 = ADVANCED_FACE ( 'NONE', ( #12863 ), #1200, .T. ) ;
#11238 = VERTEX_POINT ( 'NONE', #4740 ) ;
#11239 = EDGE_CURVE ( 'NONE', #7126, #12183, #4315, .T. ) ;
#11240 = DIRECTION ( 'NONE',  ( 0.000000000000000000, 0.000000000000000000, -1.000000000000000000 ) ) ;
#11241 = DIRECTION ( 'NONE',  ( -1.000000000000000000, -0.000000000000000000, -0.000000000000000000 ) ) ;
#11242 = CARTESIAN_POINT ( 'NONE',  ( 2.789999999999999147, -15.04425356660774682, 20.70663861606266209 ) ) ;
#11243 = LINE ( 'NONE', #4333, #6915 ) ;
#11244 = AXIS2_PLACEMENT_3D ( 'NONE', #4115, #8794, #2959 ) ;
#11245 = AXIS2_PLACEMENT_3D ( 'NONE', #10805, #8408, #5210 ) ;
#11246 = EDGE_LOOP ( 'NONE', ( #13443, #2486, #13140, #12647 ) ) ;
#11247 = DIRECTION ( 'NONE',  ( 0.000000000000000000, 0.000000000000000000, 1.000000000000000000 ) ) ;
#11248 = CARTESIAN_POINT ( 'NONE',  ( 2.765633920072236407, -2.336989772644440855, 24.63872515616082026 ) ) ;
#11249 = VERTEX_POINT ( 'NONE', #15203 ) ;
#11250 = EDGE_LOOP ( 'NONE', ( #8524, #430, #13125, #11335 ) ) ;
#11251 = LINE ( 'NONE', #4555, #13454 ) ;
#11252 = EDGE_CURVE ( 'NONE', #1565, #11809, #2009, .T. ) ;
#11253 = DIRECTION ( 'NONE',  ( 0.000000000000000000, 0.000000000000000000, 1.000000000000000000 ) ) ;
#11254 = ADVANCED_FACE ( 'NONE', ( #7188 ), #7116, .F. ) ;
#11255 = EDGE_CURVE ( 'NONE', #3709, #1757, #4817, .T. ) ;
#11256 = ORIENTED_EDGE ( 'NONE', *, *, #7954, .F. ) ;
#11257 = CARTESIAN_POINT ( 'NONE',  ( 0.000000000000000000, 7.739906618939895289, -10.88091150984218380 ) ) ;
#11258 = AXIS2_PLACEMENT_3D ( 'NONE', #6896, #191, #4602 ) ;
#11259 = AXIS2_PLACEMENT_3D ( 'NONE', #12023, #1502, #332 ) ;
#11260 = ORIENTED_EDGE ( 'NONE', *, *, #10030, .T. ) ;
#11261 = CARTESIAN_POINT ( 'NONE',  ( -14.40394475573011945, -10.79473832354794283, -3.000000000000000000 ) ) ;
#11262 = DIRECTION ( 'NONE',  ( 0.000000000000000000, 0.000000000000000000, 1.000000000000000000 ) ) ;
#11263 = ORIENTED_EDGE ( 'NONE', *, *, #13199, .F. ) ;
#11264 = B_SPLINE_CURVE_WITH_KNOTS ( 'NONE', 3,
 ( #11109, #1590, #1442, #9965, #14665, #2818 ),
 .UNSPECIFIED., .F., .F.,
 ( 4, 2, 4 ),
 ( 4.462636732861906317E-07, 0.001879885066975067612, 0.003759323870276849028 ),
 .UNSPECIFIED. ) ;
#11265 = CARTESIAN_POINT ( 'NONE',  ( 2.030753603471114666, 12.98165646470082457, 24.32906614999620132 ) ) ;
#11266 = CARTESIAN_POINT ( 'NONE',  ( 2.718184749312774429, -25.22524549359948409, -2.576941577947671647 ) ) ;
#11267 = B_SPLINE_CURVE_WITH_KNOTS ( 'NONE', 3,
 ( #856, #4324, #4553, #10314, #2014, #7929 ),
 .UNSPECIFIED., .F., .F.,
 ( 4, 2, 4 ),
 ( 2.586195665722962057E-07, 0.001878649493629687504, 0.003757040367692802973 ),
 .UNSPECIFIED. ) ;
#11268 = ORIENTED_EDGE ( 'NONE', *, *, #1931, .T. ) ;
#11269 = VERTEX_POINT ( 'NONE', #2573 ) ;
#11270 = CARTESIAN_POINT ( 'NONE',  ( 0.8291131470075423504, 24.44424927289185945, 12.96989951879416125 ) ) ;
#11271 = CIRCLE ( 'NONE', #13733, 17.95481323787947403 ) ;
#11272 = DIRECTION ( 'NONE',  ( -1.000000000000000000, 0.000000000000000000, -0.000000000000000000 ) ) ;
#11273 = LINE ( 'NONE', #747, #6313 ) ;
#11274 = DIRECTION ( 'NONE',  ( 1.000000000000000000, 0.000000000000000000, -2.710505431213761085E-17 ) ) ;
#11275 = APPLICATION_PROTOCOL_DEFINITION ( 'draft international standard', 'automotive_design', 1998, #14709 ) ;
#11276 = DIRECTION ( 'NONE',  ( 1.000000000000000000, 0.000000000000000000, 0.000000000000000000 ) ) ;
#11277 = EDGE_CURVE ( 'NONE', #14161, #4113, #3472, .T. ) ;
#11278 = CARTESIAN_POINT ( 'NONE',  ( 0.000000000000000000, 7.739906618939707883, 13.40591150984229252 ) ) ;
#11279 = EDGE_LOOP ( 'NONE', ( #1693, #2286, #4187, #12765 ) ) ;
#11280 = CARTESIAN_POINT ( 'NONE',  ( 0.000000000000000000, 0.000000000000000000, -0.8000000000000000444 ) ) ;
#11281 = CYLINDRICAL_SURFACE ( 'NONE', #4476, 2.524999999999995914 ) ;
#11282 = AXIS2_PLACEMENT_3D ( 'NONE', #5179, #4000, #3850 ) ;
#11283 = DIRECTION ( 'NONE',  ( 1.576560579138138762E-17, -1.359337748750801608E-17, 1.000000000000000000 ) ) ;
#11284 = ADVANCED_FACE ( 'NONE', ( #11098 ), #1656, .T. ) ;
#11285 = B_SPLINE_CURVE_WITH_KNOTS ( 'NONE', 3,
 ( #11087, #9935, #6560, #10090, #4256, #8931 ),
 .UNSPECIFIED., .F., .F.,
 ( 4, 2, 4 ),
 ( 2.586195665723156346E-07, 0.001878649493629684468, 0.003757040367692796902 ),
 .UNSPECIFIED. ) ;
#11286 = EDGE_LOOP ( 'NONE', ( #10336, #7535, #2210, #232, #2888, #11931, #10540 ) ) ;
#11287 = CARTESIAN_POINT ( 'NONE',  ( 2.783025342027733995, 5.408388659524090869, 23.92335783895639523 ) ) ;
#11288 = LINE ( 'NONE', #3068, #4073 ) ;
#11289 = ORIENTED_EDGE ( 'NONE', *, *, #14220, .F. ) ;
#11290 = ORIENTED_EDGE ( 'NONE', *, *, #8609, .T. ) ;
#11291 = LINE ( 'NONE', #2143, #10977 ) ;
#11292 = DIRECTION ( 'NONE',  ( -1.000000000000000000, 0.000000000000000000, 0.000000000000000000 ) ) ;
#11293 = CARTESIAN_POINT ( 'NONE',  ( 1.250000000000001110, 0.000000000000000000, 0.000000000000000000 ) ) ;
#11294 = CARTESIAN_POINT ( 'NONE',  ( 0.000000000000000000, 0.000000000000000000, 0.000000000000000000 ) ) ;
#11295 = AXIS2_PLACEMENT_3D ( 'NONE', #4284, #1987, #12346 ) ;
#11296 = DIRECTION ( 'NONE',  ( 0.000000000000000000, 0.000000000000000000, 1.000000000000000000 ) ) ;
#11297 = DIRECTION ( 'NONE',  ( 0.000000000000000000, 0.000000000000000000, 1.000000000000000000 ) ) ;
#11298 = CARTESIAN_POINT ( 'NONE',  ( 1.039999999999997815, 27.68468304288265003, -4.633866840648637186 ) ) ;
#11299 = ADVANCED_FACE ( 'NONE', ( #12256 ), #13384, .T. ) ;
#11300 = ORIENTED_EDGE ( 'NONE', *, *, #14481, .F. ) ;
#11301 = CARTESIAN_POINT ( 'NONE',  ( 2.508169649284527125, 15.84037596932108194, 3.072260951847586963 ) ) ;
#11302 = DIRECTION ( 'NONE',  ( 0.000000000000000000, 0.000000000000000000, -1.000000000000000000 ) ) ;
#11303 = ORIENTED_EDGE ( 'NONE', *, *, #8580, .T. ) ;
#11304 = ORIENTED_EDGE ( 'NONE', *, *, #10686, .F. ) ;
#11305 = VERTEX_POINT ( 'NONE', #5363 ) ;
#11306 = EDGE_LOOP ( 'NONE', ( #9419, #14108, #2330, #8477 ) ) ;
#11307 = DIRECTION ( 'NONE',  ( 0.000000000000000000, 0.000000000000000000, 1.000000000000000000 ) ) ;
#11308 = ADVANCED_FACE ( 'NONE', ( #1573, #10943 ), #13174, .T. ) ;
#11309 = CARTESIAN_POINT ( 'NONE',  ( 0.000000000000000000, 0.000000000000000000, 5.500000000000000000 ) ) ;
#11310 = EDGE_CURVE ( 'NONE', #6202, #3359, #12402, .T. ) ;
#11311 = DIRECTION ( 'NONE',  ( 5.782411586589355667E-16, 1.000000000000000000, 0.000000000000000000 ) ) ;
#11312 = CARTESIAN_POINT ( 'NONE',  ( 0.1882238782932339760, -19.18368891937503307, 17.47009390565483855 ) ) ;
#11313 = ORIENTED_EDGE ( 'NONE', *, *, #6102, .F. ) ;
#11314 = CARTESIAN_POINT ( 'NONE',  ( 1.394999999999998685, 27.68468304288265358, -4.633866840648637186 ) ) ;
#11315 = DIRECTION ( 'NONE',  ( -1.000000000000000000, -0.000000000000000000, -0.000000000000000000 ) ) ;
#11316 = DIRECTION ( 'NONE',  ( 1.000000000000000000, 0.000000000000000000, 0.000000000000000000 ) ) ;
#11317 = CARTESIAN_POINT ( 'NONE',  ( 4.000000000000000888, 4.898587196589413815E-16, 7.799999999999990052 ) ) ;
#11318 = EDGE_LOOP ( 'NONE', ( #193, #5515 ) ) ;
#11319 = CARTESIAN_POINT ( 'NONE',  ( 65.21556745095632834, 33.50594455047664866, 2.000000000000000000 ) ) ;
#11320 = DIRECTION ( 'NONE',  ( 0.000000000000000000, 0.000000000000000000, -1.000000000000000000 ) ) ;
#11321 = ORIENTED_EDGE ( 'NONE', *, *, #11173, .T. ) ;
#11322 = ORIENTED_EDGE ( 'NONE', *, *, #5616, .T. ) ;
#11323 = FACE_OUTER_BOUND ( 'NONE', #14857, .T. ) ;
#11324 = FILL_AREA_STYLE ('',( #13558 ) ) ;
#11325 = CARTESIAN_POINT ( 'NONE',  ( 1.394999999999999574, -20.02152543075331081, -19.67366047555552555 ) ) ;
#11326 = VERTEX_POINT ( 'NONE', #6341 ) ;
#11327 = EDGE_CURVE ( 'NONE', #3935, #1149, #3087, .T. ) ;
#11328 = DIRECTION ( 'NONE',  ( 1.000000000000000000, 0.000000000000000000, 0.000000000000000000 ) ) ;
#11329 = ORIENTED_EDGE ( 'NONE', *, *, #6384, .F. ) ;
#11330 = CARTESIAN_POINT ( 'NONE',  ( 8.000000000000000000, 0.000000000000000000, 0.000000000000000000 ) ) ;
#11331 = CARTESIAN_POINT ( 'NONE',  ( 0.02531912748679129854, -9.232963481057844035, 11.36963888406684298 ) ) ;
#11332 = ORIENTED_EDGE ( 'NONE', *, *, #1782, .F. ) ;
#11333 = CARTESIAN_POINT ( 'NONE',  ( 1.039999999999996039, 19.67366047555559305, -20.02152543075323976 ) ) ;
#11334 = DIRECTION ( 'NONE',  ( 0.000000000000000000, 0.000000000000000000, 1.000000000000000000 ) ) ;
#11335 = ORIENTED_EDGE ( 'NONE', *, *, #10555, .T. ) ;
#11336 = EDGE_CURVE ( 'NONE', #13280, #9067, #4016, .T. ) ;
#11337 = AXIS2_PLACEMENT_3D ( 'NONE', #6966, #15211, #2438 ) ;
#11338 = EDGE_CURVE ( 'NONE', #4228, #4155, #522, .T. ) ;
#11339 = ORIENTED_EDGE ( 'NONE', *, *, #5998, .F. ) ;
#11340 = CARTESIAN_POINT ( 'NONE',  ( 2.604434325169354913, 2.851997810081644769, 25.77772010606606301 ) ) ;
#11341 = DIRECTION ( 'NONE',  ( -1.000000000000000000, 0.000000000000000000, 0.000000000000000000 ) ) ;
#11342 = CARTESIAN_POINT ( 'NONE',  ( 93.34550147531103903, 3.654933296868752457, 4.000000000000000000 ) ) ;
#11343 = CARTESIAN_POINT ( 'NONE',  ( 0.1882239080259289210, -5.251266773802552024, 25.40949241676352344 ) ) ;
#11344 = SHAPE_DEFINITION_REPRESENTATION ( #4819, #14263 ) ;
#11345 = B_SPLINE_CURVE_WITH_KNOTS ( 'NONE', 3,
 ( #6956, #11710, #4897, #11634, #23, #7031 ),
 .UNSPECIFIED., .F., .F.,
 ( 4, 2, 4 ),
 ( 4.462636695653044375E-07, 0.001879885036799765685, 0.003759323809929966155 ),
 .UNSPECIFIED. ) ;
#11346 = CARTESIAN_POINT ( 'NONE',  ( 2.789999999999999147, 18.28042085475301093, -15.74360496233361673 ) ) ;
#11347 = CARTESIAN_POINT ( 'NONE',  ( 2.787323717450090221, 13.26666194250901931, -5.214906618938620397 ) ) ;
#11348 = EDGE_LOOP ( 'NONE', ( #14826, #3719, #3640, #6555 ) ) ;
#11350 = AXIS2_PLACEMENT_3D ( 'NONE', #5691, #1146, #3673 ) ;
#11349 = FACE_OUTER_BOUND ( 'NONE', #12773, .T. ) ;
#11351 = CARTESIAN_POINT ( 'NONE',  ( -10.00000000000000000, 0.000000000000000000, 0.000000000000000000 ) ) ;
#11352 = EDGE_CURVE ( 'NONE', #5795, #11474, #8967, .T. ) ;
#11353 = CARTESIAN_POINT ( 'NONE',  ( 1.039999999999996261, -17.29145405592685592, -4.835383649608655077 ) ) ;
#11354 = ADVANCED_FACE ( 'NONE', ( #329 ), #488, .F. ) ;
#11355 = ORIENTED_EDGE ( 'NONE', *, *, #8116, .T. ) ;
#11356 = EDGE_CURVE ( 'NONE', #3172, #7470, #1500, .T. ) ;
#11357 = CYLINDRICAL_SURFACE ( 'NONE', #142, 8.400000000000000355 ) ;
#11358 = CARTESIAN_POINT ( 'NONE',  ( 2.789999999999999591, 12.51294990530046292, -20.85230829256839513 ) ) ;
#11359 = VERTEX_POINT ( 'NONE', #13488 ) ;
#11360 = ORIENTED_EDGE ( 'NONE', *, *, #3329, .T. ) ;
#11361 = CARTESIAN_POINT ( 'NONE',  ( 2.789999999999999147, 19.64056340710875048, -14.55412442567624609 ) ) ;
#11362 = FACE_OUTER_BOUND ( 'NONE', #266, .T. ) ;
#11363 = ORIENTED_EDGE ( 'NONE', *, *, #1916, .F. ) ;
#11364 = DIRECTION ( 'NONE',  ( 1.000000000000000000, 0.000000000000000000, 0.000000000000000000 ) ) ;
#11365 = CYLINDRICAL_SURFACE ( 'NONE', #14852, 2.524999999999999467 ) ;
#11366 = CARTESIAN_POINT ( 'NONE',  ( 1.749999999999999778, 0.000000000000000000, 0.000000000000000000 ) ) ;
#11367 = ADVANCED_FACE ( 'NONE', ( #2960, #7577, #13406, #8640, #14419, #7648, #13256, #3887 ), #12092, .T. ) ;
#11368 = DIRECTION ( 'NONE',  ( 1.000000000000000000, 0.000000000000000000, 0.000000000000000000 ) ) ;
#11369 = CARTESIAN_POINT ( 'NONE',  ( 2.789999999999999147, -13.87420763704359850, -1.948757464274317508 ) ) ;
#11370 = VERTEX_POINT ( 'NONE', #11177 ) ;
#11371 = DIRECTION ( 'NONE',  ( 0.000000000000000000, 0.000000000000000000, 1.000000000000000000 ) ) ;
#11372 = CARTESIAN_POINT ( 'NONE',  ( 5.999999999999999112, 7.347880794884118750E-16, 1.395000000000000462 ) ) ;
#11373 = VERTEX_POINT ( 'NONE', #6263 ) ;
#11374 = VERTEX_POINT ( 'NONE', #408 ) ;
#11375 = ORIENTED_EDGE ( 'NONE', *, *, #4321, .F. ) ;
#11376 = ORIENTED_EDGE ( 'NONE', *, *, #10150, .F. ) ;
#11377 = CARTESIAN_POINT ( 'NONE',  ( 2.030753605846571386, 27.31305418910209326, 3.797885586973312133 ) ) ;
#11378 = FACE_OUTER_BOUND ( 'NONE', #4750, .T. ) ;
#11379 = PRESENTATION_LAYER_ASSIGNMENT (  '', '', ( #8429 ) ) ;
#11380 = CARTESIAN_POINT ( 'NONE',  ( 0.02531912748679129854, -9.232963481057844035, 11.36963888406684298 ) ) ;
#11381 = EDGE_LOOP ( 'NONE', ( #206, #7865, #11730, #8841 ) ) ;
#11382 = VECTOR ( 'NONE', #7409, 1000.000000000000000 ) ;
#11383 = CARTESIAN_POINT ( 'NONE',  ( 0.7589665089996495695, 24.80232951178378187, 12.05173163741731202 ) ) ;
#11384 = DIRECTION ( 'NONE',  ( 0.000000000000000000, 0.000000000000000000, 1.000000000000000000 ) ) ;
#11385 = LINE ( 'NONE', #14720, #11598 ) ;
#11386 = AXIS2_PLACEMENT_3D ( 'NONE', #5883, #9397, #7020 ) ;
#11387 = CIRCLE ( 'NONE', #1327, 3.799999999999999378 ) ;
#11388 = ORIENTED_EDGE ( 'NONE', *, *, #13390, .F. ) ;
#11389 = CYLINDRICAL_SURFACE ( 'NONE', #13386, 17.95481323787947403 ) ;
#11390 = CARTESIAN_POINT ( 'NONE',  ( 0.02436607992776325046, -24.15498966839958683, -5.391175441198872598 ) ) ;
#11391 = ORIENTED_EDGE ( 'NONE', *, *, #13327, .T. ) ;
#11392 = VERTEX_POINT ( 'NONE', #12488 ) ;
#11393 = CYLINDRICAL_SURFACE ( 'NONE', #5303, 6.000000000000000888 ) ;
#11394 = AXIS2_PLACEMENT_3D ( 'NONE', #3869, #8550, #14086 ) ;
#11395 = ORIENTED_EDGE ( 'NONE', *, *, #3451, .T. ) ;
#11396 = VECTOR ( 'NONE', #6383, 1000.000000000000000 ) ;
#11397 = CYLINDRICAL_SURFACE ( 'NONE', #12243, 10.00000000000000000 ) ;
#11398 = EDGE_LOOP ( 'NONE', ( #5970, #4052, #1512, #1354 ) ) ;
#11399 = FACE_OUTER_BOUND ( 'NONE', #11306, .T. ) ;
#11400 = DIRECTION ( 'NONE',  ( 0.1305261922200521840, -0.9914448613738103822, 0.000000000000000000 ) ) ;
#11401 = ORIENTED_EDGE ( 'NONE', *, *, #5060, .F. ) ;
#11402 = B_SPLINE_CURVE_WITH_KNOTS ( 'NONE', 3,
 ( #6586, #11184, #13795, #13645, #11266, #6804 ),
 .UNSPECIFIED., .F., .F.,
 ( 4, 2, 4 ),
 ( 4.462636732861209103E-07, 0.001879885066975070214, 0.003759323870276854232 ),
 .UNSPECIFIED. ) ;
#11403 = DIRECTION ( 'NONE',  ( -1.000000000000000000, -0.000000000000000000, 0.000000000000000000 ) ) ;
#11404 = EDGE_CURVE ( 'NONE', #13491, #8235, #3566, .T. ) ;
#11405 = CARTESIAN_POINT ( 'NONE',  ( 1.039999999999996261, 4.458161950358501713, 17.39253030560843172 ) ) ;
#11406 = B_SPLINE_CURVE_WITH_KNOTS ( 'NONE', 3,
 ( #3671, #7135, #200, #11806, #3515, #6133, #115, #8202 ),
 .UNSPECIFIED., .F., .F.,
 ( 4, 2, 2, 4 ),
 ( 4.663089536324781369E-07, 0.001898630414085404096, 0.002847712466651293635, 0.003796794519217182740 ),
 .UNSPECIFIED. ) ;
#11407 = VERTEX_POINT ( 'NONE', #10175 ) ;
#11408 = PRESENTATION_LAYER_ASSIGNMENT (  '', '', ( #15102 ) ) ;
#11409 = ADVANCED_FACE ( 'NONE', ( #6571 ), #6270, .T. ) ;
#11410 = VERTEX_POINT ( 'NONE', #12556 ) ;
#11411 = DIRECTION ( 'NONE',  ( 1.000000000000000000, 1.734723475976807341E-16, -6.938893903907229364E-16 ) ) ;
#11412 = CARTESIAN_POINT ( 'NONE',  ( 2.740856711021125047, -13.98777112126107802, 5.263533129984309333 ) ) ;
#11413 = CARTESIAN_POINT ( 'NONE',  ( -10.40394475573011945, -10.79473832354794460, -5.000000000000000000 ) ) ;
#11414 = DIRECTION ( 'NONE',  ( 0.9148936170212769170, 0.4036950204470268755, -0.000000000000000000 ) ) ;
#11415 = CARTESIAN_POINT ( 'NONE',  ( 2.789999999999999147, 24.04302995059966364, 1.991882183130384121 ) ) ;
#11416 = CARTESIAN_POINT ( 'NONE',  ( 2.789999999999999147, 12.98979500319701508, -5.249430348645618416 ) ) ;
#11417 = VECTOR ( 'NONE', #11551, 1000.000000000000114 ) ;
#11418 = ADVANCED_FACE ( 'NONE', ( #10102 ), #12405, .F. ) ;
#11419 = ORIENTED_EDGE ( 'NONE', *, *, #12918, .T. ) ;
#11420 = CARTESIAN_POINT ( 'NONE',  ( 1.749999999999998002, 0.000000000000000000, 0.000000000000000000 ) ) ;
#11421 = AXIS2_PLACEMENT_3D ( 'NONE', #13058, #70, #1313 ) ;
#11422 = EDGE_CURVE ( 'NONE', #6526, #2853, #1350, .T. ) ;
#11423 = CARTESIAN_POINT ( 'NONE',  ( -7.682766964941417370E-14, -9.515416771311052457, -22.38018801136486502 ) ) ;
#11424 = DIRECTION ( 'NONE',  ( 0.000000000000000000, 0.000000000000000000, 1.000000000000000000 ) ) ;
#11425 = ORIENTED_EDGE ( 'NONE', *, *, #11227, .F. ) ;
#11426 = CYLINDRICAL_SURFACE ( 'NONE', #1877, 28.06981291497571362 ) ;
#11427 = CARTESIAN_POINT ( 'NONE',  ( 1.749999999999998002, 4.633866840649310426, -27.68468304288254345 ) ) ;
#11428 = ORIENTED_EDGE ( 'NONE', *, *, #13871, .F. ) ;
#11429 = VERTEX_POINT ( 'NONE', #1884 ) ;
#11430 = FACE_OUTER_BOUND ( 'NONE', #10376, .T. ) ;
#11431 = AXIS2_PLACEMENT_3D ( 'NONE', #15054, #6751, #903 ) ;
#11432 = DIRECTION ( 'NONE',  ( 0.000000000000000000, 0.000000000000000000, 1.000000000000000000 ) ) ;
#11433 = EDGE_LOOP ( 'NONE', ( #11870, #12214, #1251, #5244 ) ) ;
#11434 = DIRECTION ( 'NONE',  ( 1.000000000000000000, 0.000000000000000000, 0.000000000000000000 ) ) ;
#11435 = CARTESIAN_POINT ( 'NONE',  ( 8.000000000000000000, 0.000000000000000000, 0.000000000000000000 ) ) ;
#11436 = DIRECTION ( 'NONE',  ( -1.000000000000000000, -0.000000000000000000, -0.000000000000000000 ) ) ;
#11437 = EDGE_CURVE ( 'NONE', #10601, #5949, #8942, .T. ) ;
#11438 = CARTESIAN_POINT ( 'NONE',  ( 2.789999999999999147, 13.40591150984237245, -7.739906618939567551 ) ) ;
#11439 = CARTESIAN_POINT ( 'NONE',  ( 0.02531912748464718033, -9.232963481057685939, -11.36963888406697087 ) ) ;
#11440 = EDGE_CURVE ( 'NONE', #15071, #3292, #14869, .T. ) ;
#11441 = ORIENTED_EDGE ( 'NONE', *, *, #3135, .T. ) ;
#11442 = AXIS2_PLACEMENT_3D ( 'NONE', #5325, #13532, #3003 ) ;
#11443 = CARTESIAN_POINT ( 'NONE',  ( 2.021362756903528179, 17.00993931356761379, 4.022333916463652237 ) ) ;
#11444 = AXIS2_PLACEMENT_3D ( 'NONE', #10934, #12802, #3880 ) ;
#11445 = DIRECTION ( 'NONE',  ( 1.000000000000000000, 0.000000000000000000, 0.000000000000000000 ) ) ;
#11446 = ORIENTED_EDGE ( 'NONE', *, *, #8228, .T. ) ;
#11447 = STYLED_ITEM ( 'NONE', ( #13916 ), #1226 ) ;
#11448 = CIRCLE ( 'NONE', #4835, 2.000000000000003109 ) ;
#11449 = ADVANCED_FACE ( 'NONE', ( #4265 ), #6651, .T. ) ;
#11450 =( NAMED_UNIT ( * ) PLANE_ANGLE_UNIT ( ) SI_UNIT ( $, .RADIAN. ) );
#11451 = B_SPLINE_CURVE_WITH_KNOTS ( 'NONE', 3,
 ( #11147, #1783, #8847, #6318 ),
 .UNSPECIFIED., .F., .F.,
 ( 4, 4 ),
 ( 0.005258139959819238193, 0.005342776758202895035 ),
 .UNSPECIFIED. ) ;
#11452 = VERTEX_POINT ( 'NONE', #14797 ) ;
#11453 = ORIENTED_EDGE ( 'NONE', *, *, #1399, .F. ) ;
#11454 = ORIENTED_EDGE ( 'NONE', *, *, #14259, .F. ) ;
#11455 = LINE ( 'NONE', #1008, #1892 ) ;
#11456 = CARTESIAN_POINT ( 'NONE',  ( 1.000000000000000000, -5.408326913195983465, -0.8000000000000000444 ) ) ;
#11457 = FACE_OUTER_BOUND ( 'NONE', #8038, .T. ) ;
#11458 =( REPRESENTATION_RELATIONSHIP ('NONE','NONE', #12685, #4172 ) REPRESENTATION_RELATIONSHIP_WITH_TRANSFORMATION ( #5823 )SHAPE_REPRESENTATION_RELATIONSHIP( ) );
#11459 = AXIS2_PLACEMENT_3D ( 'NONE', #8083, #12757, #2239 ) ;
#11460 = CARTESIAN_POINT ( 'NONE',  ( 1.149999999999998135, 0.000000000000000000, -4.100000000000000533 ) ) ;
#11461 = CIRCLE ( 'NONE', #4614, 2.524999999999995914 ) ;
#11462 = EDGE_LOOP ( 'NONE', ( #4245, #11185, #4087, #14250 ) ) ;
#11463 = CIRCLE ( 'NONE', #2179, 4.000000000000000888 ) ;
#11464 = CARTESIAN_POINT ( 'NONE',  ( 2.789999999999999147, -12.98979500319690317, -5.249430348645892863 ) ) ;
#11465 = DIRECTION ( 'NONE',  ( 1.000000000000000000, 0.000000000000000000, 0.000000000000000000 ) ) ;
#11466 = CARTESIAN_POINT ( 'NONE',  ( 0.000000000000000000, -7.909232158574988958, 24.34211360614297348 ) ) ;
#11467 = EDGE_CURVE ( 'NONE', #6969, #14971, #3115, .T. ) ;
#11468 = VECTOR ( 'NONE', #10883, 1000.000000000000000 ) ;
#11469 = ORIENTED_EDGE ( 'NONE', *, *, #15112, .T. ) ;
#11470 = MECHANICAL_DESIGN_GEOMETRIC_PRESENTATION_REPRESENTATION (  '', ( #7558 ), #4583 ) ;
#11471 = CARTESIAN_POINT ( 'NONE',  ( 4.000000000000000000, 4.898587196589412829E-16, 5.500000000000000000 ) ) ;
#11472 = DIRECTION ( 'NONE',  ( 0.000000000000000000, 0.000000000000000000, -1.000000000000000000 ) ) ;
#11473 = CIRCLE ( 'NONE', #15181, 5.899999999999999467 ) ;
#11474 = VERTEX_POINT ( 'NONE', #12702 ) ;
#11475 = ORIENTED_EDGE ( 'NONE', *, *, #6088, .T. ) ;
#11476 = AXIS2_PLACEMENT_3D ( 'NONE', #9032, #5504, #4198 ) ;
#11477 = CARTESIAN_POINT ( 'NONE',  ( 10.00000000000000178, -1.390791565672601315, 6.000000000000005329 ) ) ;
#11478 = EDGE_LOOP ( 'NONE', ( #7475, #14474 ) ) ;
#11479 = EDGE_CURVE ( 'NONE', #14329, #9661, #1466, .T. ) ;
#11480 = AXIS2_PLACEMENT_3D ( 'NONE', #137, #9378, #2539 ) ;
#11481 = LINE ( 'NONE', #15104, #10285 ) ;
#11482 = EDGE_CURVE ( 'NONE', #6574, #12986, #6794, .T. ) ;
#11483 = CARTESIAN_POINT ( 'NONE',  ( 2.601776144743014108, 10.68696068830440815, -23.64332819722370260 ) ) ;
#11484 = CARTESIAN_POINT ( 'NONE',  ( 2.789999999999999147, 12.52067188844351442, 20.62201879784917935 ) ) ;
#11485 = VECTOR ( 'NONE', #6957, 1000.000000000000000 ) ;
#11486 = ORIENTED_EDGE ( 'NONE', *, *, #14408, .T. ) ;
#11487 = LINE ( 'NONE', #3344, #8019 ) ;
#11488 = ORIENTED_EDGE ( 'NONE', *, *, #11950, .F. ) ;
#11489 = EDGE_LOOP ( 'NONE', ( #979, #14567, #12679, #1364 ) ) ;
#11490 = CARTESIAN_POINT ( 'NONE',  ( 1.749999999999998002, 4.147968289691286614, 27.76164181293053090 ) ) ;
#11491 = DIRECTION ( 'NONE',  ( 0.000000000000000000, 0.000000000000000000, 1.000000000000000000 ) ) ;
#11492 = EDGE_CURVE ( 'NONE', #11124, #1547, #4801, .T. ) ;
#11493 = CARTESIAN_POINT ( 'NONE',  ( -11.52599798030746037, -13.27615371759915242, -3.873810994203807765E-15 ) ) ;
#11494 = CARTESIAN_POINT ( 'NONE',  ( 2.700582527824513690, 14.29395843996386262, 5.279841123860917307 ) ) ;
#11495 = VECTOR ( 'NONE', #7902, 1000.000000000000000 ) ;
#11496 = DIRECTION ( 'NONE',  ( 1.000000000000000000, -0.000000000000000000, -0.000000000000000000 ) ) ;
#11497 = EDGE_CURVE ( 'NONE', #6090, #11305, #13374, .T. ) ;
#11498 = FACE_BOUND ( 'NONE', #5753, .T. ) ;
#11499 = ORIENTED_EDGE ( 'NONE', *, *, #4556, .F. ) ;
#11500 = CARTESIAN_POINT ( 'NONE',  ( 0.000000000000000000, 0.000000000000000000, 1.395000000000000462 ) ) ;
#11501 = DIRECTION ( 'NONE',  ( 0.000000000000000000, 0.000000000000000000, 1.000000000000000000 ) ) ;
#11502 = CARTESIAN_POINT ( 'NONE',  ( 93.49175023922396122, 0.6585002008270834928, 6.000000000000000000 ) ) ;
#11503 = ORIENTED_EDGE ( 'NONE', *, *, #5817, .T. ) ;
#11504 = AXIS2_PLACEMENT_3D ( 'NONE', #10750, #9303, #5981 ) ;
#11505 = AXIS2_PLACEMENT_3D ( 'NONE', #13806, #11790, #11718 ) ;
#11506 = DIRECTION ( 'NONE',  ( 0.000000000000000000, 0.8660254037844433705, -0.4999999999999918954 ) ) ;
#11507 = PLANE ( 'NONE',  #11431 ) ;
#11508 = ORIENTED_EDGE ( 'NONE', *, *, #630, .F. ) ;
#11509 = VERTEX_POINT ( 'NONE', #8864 ) ;
#11510 = CARTESIAN_POINT ( 'NONE',  ( 2.789999999999999147, -20.70663861606260170, -15.04425356660783031 ) ) ;
#11511 = CARTESIAN_POINT ( 'NONE',  ( 2.777258977888996672, -13.49735377262296332, -5.214906618939849636 ) ) ;
#11512 = ADVANCED_FACE ( 'NONE', ( #5431 ), #7878, .F. ) ;
#11513 = ORIENTED_EDGE ( 'NONE', *, *, #5488, .F. ) ;
#11514 = CARTESIAN_POINT ( 'NONE',  ( 0.000000000000000000, -15.04425356660744839, -20.70663861606288236 ) ) ;
#11515 = CARTESIAN_POINT ( 'NONE',  ( 2.788134175425139194, -20.90825775245756191, -12.51925356660783528 ) ) ;
#11516 = DIRECTION ( 'NONE',  ( -0.000000000000000000, -0.000000000000000000, 1.000000000000000000 ) ) ;
#11517 = CARTESIAN_POINT ( 'NONE',  ( 72.68384697807672978, 11.35494834827056110, 2.999999999999999112 ) ) ;
#11518 = CARTESIAN_POINT ( 'NONE',  ( 1.749999999999999778, -17.29145405592685236, -4.835383649608663070 ) ) ;
#11519 = VECTOR ( 'NONE', #9608, 1000.000000000000000 ) ;
#11520 = ORIENTED_EDGE ( 'NONE', *, *, #10988, .T. ) ;
#11521 = CARTESIAN_POINT ( 'NONE',  ( 93.63799900313688340, -2.337932895214618778, 6.000000000000000000 ) ) ;
#11522 = ADVANCED_FACE ( 'NONE', ( #3334 ), #11393, .F. ) ;
#11523 = CARTESIAN_POINT ( 'NONE',  ( 2.321707774797442170, -4.824281976789052351, -0.8000000000000000444 ) ) ;
#11524 = ORIENTED_EDGE ( 'NONE', *, *, #5906, .T. ) ;
#11525 = ORIENTED_EDGE ( 'NONE', *, *, #13306, .T. ) ;
#11526 = ORIENTED_EDGE ( 'NONE', *, *, #9004, .F. ) ;
#11527 = ORIENTED_EDGE ( 'NONE', *, *, #11812, .T. ) ;
#11528 = AXIS2_PLACEMENT_3D ( 'NONE', #13905, #1224, #1068 ) ;
#11529 = CARTESIAN_POINT ( 'NONE',  ( 1.749999999999999778, -12.83329210556841282, 12.55714665599981927 ) ) ;
#11530 = EDGE_CURVE ( 'NONE', #4613, #4354, #12149, .T. ) ;
#11531 = PRESENTATION_STYLE_ASSIGNMENT (( #9232 ) ) ;
#11532 = EDGE_CURVE ( 'NONE', #7859, #6954, #1114, .T. ) ;
#11533 = PLANE ( 'NONE',  #7806 ) ;
#11534 = UNCERTAINTY_MEASURE_WITH_UNIT (LENGTH_MEASURE( 1.000000000000000082E-05 ), #14041, 'distance_accuracy_value', 'NONE');
#11535 = CARTESIAN_POINT ( 'NONE',  ( -9.886993524391892676E-15, -14.05347802000167690, -2.096460570596322182 ) ) ;
#11536 = B_SPLINE_CURVE_WITH_KNOTS ( 'NONE', 3,
 ( #3974, #3903, #7592, #572, #14582, #9882 ),
 .UNSPECIFIED., .F., .F.,
 ( 4, 2, 4 ),
 ( 4.462636695690012598E-07, 0.001879885036799766119, 0.003759323809929963553 ),
 .UNSPECIFIED. ) ;
#11537 = ORIENTED_EDGE ( 'NONE', *, *, #4868, .T. ) ;
#11538 = DIRECTION ( 'NONE',  ( 0.000000000000000000, 0.000000000000000000, -1.000000000000000000 ) ) ;
#11539 = CARTESIAN_POINT ( 'NONE',  ( 1.039999999999998037, -4.458161950358621617, 17.39253030560839974 ) ) ;
#11540 = ADVANCED_FACE ( 'NONE', ( #11839 ), #15185, .F. ) ;
#11541 = DIRECTION ( 'NONE',  ( 0.000000000000000000, 0.000000000000000000, 1.000000000000000000 ) ) ;
#11542 = EDGE_CURVE ( 'NONE', #6646, #8949, #4560, .T. ) ;
#11543 = ORIENTED_EDGE ( 'NONE', *, *, #11668, .T. ) ;
#11544 = FACE_OUTER_BOUND ( 'NONE', #2200, .T. ) ;
#11545 = PRODUCT_DEFINITION_SHAPE ( 'NONE', 'NONE',  #7771 ) ;
#11546 = CARTESIAN_POINT ( 'NONE',  ( 0.000000000000000000, 0.000000000000000000, 4.500000000000000888 ) ) ;
#11547 = ADVANCED_FACE ( 'NONE', ( #5799 ), #4655, .T. ) ;
#11548 = VERTEX_POINT ( 'NONE', #14013 ) ;
#11549 = ORIENTED_EDGE ( 'NONE', *, *, #7856, .T. ) ;
#11550 = B_SPLINE_CURVE_WITH_KNOTS ( 'NONE', 3,
 ( #14562, #7257, #1723, #9713, #4025, #2727, #14493, #8699 ),
 .UNSPECIFIED., .F., .F.,
 ( 4, 2, 2, 4 ),
 ( 4.663089536324781899E-07, 0.001898630414085405180, 0.002847712466651292334, 0.003796794519217179704 ),
 .UNSPECIFIED. ) ;
#11551 = DIRECTION ( 'NONE',  ( -0.5416238976136773520, 0.8406209333187989463, 0.000000000000000000 ) ) ;
#11552 = EDGE_CURVE ( 'NONE', #10516, #99, #371, .T. ) ;
#11553 = ORIENTED_EDGE ( 'NONE', *, *, #6049, .T. ) ;
#11554 = B_SPLINE_CURVE_WITH_KNOTS ( 'NONE', 3,
 ( #14606, #3075, #4077, #13447 ),
 .UNSPECIFIED., .F., .F.,
 ( 4, 4 ),
 ( 0.005123713096549392838, 0.005814346476695830997 ),
 .UNSPECIFIED. ) ;
#11555 = CARTESIAN_POINT ( 'NONE',  ( 0.000000000000000000, -12.52067188844364587, 20.62201879784910119 ) ) ;
#11556 = FACE_OUTER_BOUND ( 'NONE', #7659, .T. ) ;
#11557 = CARTESIAN_POINT ( 'NONE',  ( -3.160591952521660364, -3.281206521718067037, -0.8000000000000000444 ) ) ;
#11558 = DIRECTION ( 'NONE',  ( -1.000000000000000000, -0.000000000000000000, -0.000000000000000000 ) ) ;
#11559 = ORIENTED_EDGE ( 'NONE', *, *, #13946, .T. ) ;
#11560 = CARTESIAN_POINT ( 'NONE',  ( -14.40394475573012301, -7.794738323547949932, 16.99999999999999645 ) ) ;
#11561 = CYLINDRICAL_SURFACE ( 'NONE', #6792, 2.524999999999999467 ) ;
#11562 = ORIENTED_EDGE ( 'NONE', *, *, #6507, .F. ) ;
#11563 = ORIENTED_EDGE ( 'NONE', *, *, #14002, .T. ) ;
#11564 = DIRECTION ( 'NONE',  ( 0.000000000000000000, 0.000000000000000000, 1.000000000000000000 ) ) ;
#11565 = CIRCLE ( 'NONE', #13540, 17.95481323787947403 ) ;
#11566 = CARTESIAN_POINT ( 'NONE',  ( 2.789999999999999147, 23.17675759782029843, 7.772527002114834715 ) ) ;
#11567 = DIRECTION ( 'NONE',  ( -1.000000000000000000, 0.000000000000000000, 0.000000000000000000 ) ) ;
#11568 = CARTESIAN_POINT ( 'NONE',  ( 0.5321745407694777885, -4.993157874728001211, 26.58873630738050409 ) ) ;
#11569 = DIRECTION ( 'NONE',  ( 0.000000000000000000, 0.000000000000000000, 1.000000000000000000 ) ) ;
#11570 = CARTESIAN_POINT ( 'NONE',  ( 0.02436607992776325046, -18.55949924794904504, 16.37294372382852004 ) ) ;
#11571 = VERTEX_POINT ( 'NONE', #75 ) ;
#11572 = CARTESIAN_POINT ( 'NONE',  ( 2.789999999999999147, 14.18181402625742749, 19.91106274590519121 ) ) ;
#11573 = CARTESIAN_POINT ( 'NONE',  ( 0.02436607992776238310, -12.59161484032927092, 21.30679549418627161 ) ) ;
#11574 = CARTESIAN_POINT ( 'NONE',  ( 1.749999999999998002, -12.96210679857767367, -24.89775460606847091 ) ) ;
#11575 = CARTESIAN_POINT ( 'NONE',  ( -17.28189153115278032, -8.313322929496736791, -3.715604213194723273E-15 ) ) ;
#11576 = CIRCLE ( 'NONE', #5228, 1.999999999999998890 ) ;
#11577 = VERTEX_POINT ( 'NONE', #14083 ) ;
#11578 = EDGE_CURVE ( 'NONE', #8828, #11849, #2840, .T. ) ;
#11579 = DIRECTION ( 'NONE',  ( -0.000000000000000000, -0.000000000000000000, -1.000000000000000000 ) ) ;
#11580 = PRESENTATION_STYLE_ASSIGNMENT (( #10588 ) ) ;
#11581 = EDGE_LOOP ( 'NONE', ( #8395, #1317, #4656, #9147, #10397, #5792 ) ) ;
#11582 = VERTEX_POINT ( 'NONE', #10627 ) ;
#11583 = FACE_OUTER_BOUND ( 'NONE', #6047, .T. ) ;
#11584 = DIRECTION ( 'NONE',  ( -1.445602896647338917E-16, 1.000000000000000000, -0.000000000000000000 ) ) ;
#11585 = EDGE_LOOP ( 'NONE', ( #5719, #6458, #8112, #15022 ) ) ;
#11586 = DIRECTION ( 'NONE',  ( 1.000000000000000000, 0.000000000000000000, 0.000000000000000000 ) ) ;
#11587 = DIRECTION ( 'NONE',  ( -1.000000000000000000, -0.000000000000000000, -0.000000000000000000 ) ) ;
#11588 = CYLINDRICAL_SURFACE ( 'NONE', #4979, 5.400000000000000355 ) ;
#11589 = VECTOR ( 'NONE', #6620, 1000.000000000000000 ) ;
#11590 = AXIS2_PLACEMENT_3D ( 'NONE', #10875, #8409, #3968 ) ;
#11591 = DIRECTION ( 'NONE',  ( 0.000000000000000000, -1.000000000000000000, -0.000000000000000000 ) ) ;
#11592 = FACE_OUTER_BOUND ( 'NONE', #6842, .T. ) ;
#11593 = VERTEX_POINT ( 'NONE', #11694 ) ;
#11594 = DIRECTION ( 'NONE',  ( 0.9021244663126475327, 0.4314758942051350465, -1.141265444721583757E-16 ) ) ;
#11595 = LINE ( 'NONE', #12673, #9924 ) ;
#11596 = EDGE_LOOP ( 'NONE', ( #3093, #5591, #466, #1041 ) ) ;
#11597 = ADVANCED_FACE ( 'NONE', ( #10558 ), #12916, .F. ) ;
#11598 = VECTOR ( 'NONE', #12478, 1000.000000000000000 ) ;
#11599 = ORIENTED_EDGE ( 'NONE', *, *, #4306, .T. ) ;
#11600 = ORIENTED_EDGE ( 'NONE', *, *, #8964, .T. ) ;
#11601 = EDGE_LOOP ( 'NONE', ( #10880, #3703, #792, #703 ) ) ;
#11602 = LINE ( 'NONE', #15160, #1402 ) ;
#11603 = ADVANCED_FACE ( 'NONE', ( #4723 ), #11617, .T. ) ;
#11604 = CARTESIAN_POINT ( 'NONE',  ( 0.09203962824862119141, -9.756102650610156246, -11.73065272960073457 ) ) ;
#11605 = CARTESIAN_POINT ( 'NONE',  ( 18.21994936526786901, -20.29667510578869027, 7.000000000000000000 ) ) ;
#11606 = DIRECTION ( 'NONE',  ( 0.000000000000000000, 0.000000000000000000, 1.000000000000000000 ) ) ;
#11607 = ORIENTED_EDGE ( 'NONE', *, *, #3343, .F. ) ;
#11608 = DIRECTION ( 'NONE',  ( -0.000000000000000000, -0.000000000000000000, 1.000000000000000000 ) ) ;
#11609 = EDGE_CURVE ( 'NONE', #10221, #5235, #9468, .T. ) ;
#11610 = EDGE_CURVE ( 'NONE', #6540, #11997, #2582, .T. ) ;
#11611 = DIRECTION ( 'NONE',  ( -1.000000000000000000, -0.000000000000000000, -0.000000000000000000 ) ) ;
#11612 = ORIENTED_EDGE ( 'NONE', *, *, #2538, .F. ) ;
#11613 = CARTESIAN_POINT ( 'NONE',  ( 1.250000000000000666, 5.899999999999999467, 0.000000000000000000 ) ) ;
#11614 = DIRECTION ( 'NONE',  ( 0.000000000000000000, 0.000000000000000000, 1.000000000000000000 ) ) ;
#11615 = VERTEX_POINT ( 'NONE', #14243 ) ;
#11616 = ORIENTED_EDGE ( 'NONE', *, *, #8997, .T. ) ;
#11617 = CYLINDRICAL_SURFACE ( 'NONE', #15111, 13.20000000000000284 ) ;
#11618 = EDGE_CURVE ( 'NONE', #8456, #12831, #6194, .T. ) ;
#11619 = LINE ( 'NONE', #4621, #10127 ) ;
#11620 = ORIENTED_EDGE ( 'NONE', *, *, #3602, .F. ) ;
#11621 = CARTESIAN_POINT ( 'NONE',  ( 0.000000000000000000, 0.000000000000000000, 0.000000000000000000 ) ) ;
#11622 = CARTESIAN_POINT ( 'NONE',  ( 2.765633920072238183, -18.55949924794904504, 16.37294372382852004 ) ) ;
#11623 = EDGE_CURVE ( 'NONE', #4526, #6903, #13941, .T. ) ;
#11624 = DIRECTION ( 'NONE',  ( -1.000000000000000000, -2.081668171172168513E-16, 0.000000000000000000 ) ) ;
#11625 = LINE ( 'NONE', #10489, #578 ) ;
#11626 = CIRCLE ( 'NONE', #6732, 2.524999999999999023 ) ;
#11627 = VECTOR ( 'NONE', #699, 1000.000000000000000 ) ;
#11628 = VERTEX_POINT ( 'NONE', #2552 ) ;
#11629 = CYLINDRICAL_SURFACE ( 'NONE', #6210, 2.999999999999975131 ) ;
#11630 = VECTOR ( 'NONE', #3676, 1000.000000000000227 ) ;
#11631 = ORIENTED_EDGE ( 'NONE', *, *, #11310, .F. ) ;
#11632 = ADVANCED_FACE ( 'NONE', ( #5942 ), #2257, .F. ) ;
#11633 = VERTEX_POINT ( 'NONE', #1250 ) ;
#11634 = CARTESIAN_POINT ( 'NONE',  ( 2.601776096565022289, 22.54313264455032240, -12.84621645676820201 ) ) ;
#11636 = LINE ( 'NONE', #7265, #5626 ) ;
#11635 = AXIS2_PLACEMENT_3D ( 'NONE', #1842, #2770, #14691 ) ;
#11637 = CIRCLE ( 'NONE', #3544, 28.06981291497571007 ) ;
#11638 = CARTESIAN_POINT ( 'NONE',  ( 2.697960317788777207, 5.280991956247118146, 14.31435947614544091 ) ) ;
#11639 = AXIS2_PLACEMENT_3D ( 'NONE', #14369, #3832, #9598 ) ;
#11640 = CARTESIAN_POINT ( 'NONE',  ( 80.00000000000000000, 0.000000000000000000, 3.000000000000000000 ) ) ;
#11641 = ITEM_DEFINED_TRANSFORMATION ( 'NONE', 'NONE', #7493,  #1376 ) ;
#11642 = CARTESIAN_POINT ( 'NONE',  ( 3.799999999999999378, 0.000000000000000000, 0.000000000000000000 ) ) ;
#11643 = DIRECTION ( 'NONE',  ( -1.000000000000000000, -0.000000000000000000, 0.000000000000000000 ) ) ;
#11644 = ORIENTED_EDGE ( 'NONE', *, *, #1873, .F. ) ;
#11645 = PLANE ( 'NONE',  #9295 ) ;
#11646 = DIRECTION ( 'NONE',  ( 0.000000000000000000, 0.000000000000000000, -1.000000000000000000 ) ) ;
#11647 = DIRECTION ( 'NONE',  ( 1.000000000000000000, 0.000000000000000000, 0.000000000000000000 ) ) ;
#11648 = VECTOR ( 'NONE', #2749, 1000.000000000000000 ) ;
#11649 = DIRECTION ( 'NONE',  ( 0.000000000000000000, 0.000000000000000000, 1.000000000000000000 ) ) ;
#11650 = ORIENTED_EDGE ( 'NONE', *, *, #6256, .T. ) ;
#11651 = VECTOR ( 'NONE', #13713, 1000.000000000000000 ) ;
#11652 = LINE ( 'NONE', #12082, #9478 ) ;
#11653 = EDGE_LOOP ( 'NONE', ( #2763, #9547, #10718, #1449, #13538, #11339, #14782 ) ) ;
#11654 = CARTESIAN_POINT ( 'NONE',  ( 0.000000000000000000, -12.98979500319690850, -5.249430348645889310 ) ) ;
#11655 = CARTESIAN_POINT ( 'NONE',  ( 1.749999999999999778, -17.39253030560844948, 4.458161950358431547 ) ) ;
#11656 = CARTESIAN_POINT ( 'NONE',  ( 0.4522159317772150855, 5.191253194756014544, 15.84984805378633688 ) ) ;
#11657 = CARTESIAN_POINT ( 'NONE',  ( 2.780931166827226519, -21.10834851580694504, -12.54305517365643929 ) ) ;
#11658 = DIRECTION ( 'NONE',  ( 1.000000000000000000, 0.000000000000000000, 0.000000000000000000 ) ) ;
#11659 = AXIS2_PLACEMENT_3D ( 'NONE', #3032, #12624, #9028 ) ;
#11660 = AXIS2_PLACEMENT_3D ( 'NONE', #13610, #1549, #5107 ) ;
#11661 = FACE_OUTER_BOUND ( 'NONE', #2837, .T. ) ;
#11662 = DIRECTION ( 'NONE',  ( 1.576560579138138762E-17, -1.359337748750801608E-17, 1.000000000000000000 ) ) ;
#11663 = VERTEX_POINT ( 'NONE', #7246 ) ;
#11664 = ADVANCED_FACE ( 'NONE', ( #11917 ), #6097, .T. ) ;
#11665 = DIRECTION ( 'NONE',  ( -1.000000000000000000, 0.000000000000000000, 0.000000000000000000 ) ) ;
#11666 = PRODUCT_DEFINITION_SHAPE ( 'NONE', 'NONE',  #15226 ) ;
#11667 = PLANE ( 'NONE',  #14855 ) ;
#11668 = EDGE_CURVE ( 'NONE', #7388, #5377, #8621, .T. ) ;
#11669 = ORIENTED_EDGE ( 'NONE', *, *, #4717, .T. ) ;
#11670 = AXIS2_PLACEMENT_3D ( 'NONE', #13153, #13383, #1635 ) ;
#11671 = SHAPE_REPRESENTATION_RELATIONSHIP ( 'NONE' , 'NONE' ,  #7313, #13135 ) ;
#11672 = ORIENTED_EDGE ( 'NONE', *, *, #4802, .F. ) ;
#11673 = ORIENTED_EDGE ( 'NONE', *, *, #4293, .F. ) ;
#11674 = EDGE_LOOP ( 'NONE', ( #6259, #4797, #734, #2528 ) ) ;
#11675 = FACE_BOUND ( 'NONE', #7414, .T. ) ;
#11676 = CARTESIAN_POINT ( 'NONE',  ( 8.000000000000000000, 0.000000000000000000, 0.000000000000000000 ) ) ;
#11677 = CARTESIAN_POINT ( 'NONE',  ( 80.00000000000000000, 0.000000000000000000, 7.000000000000000000 ) ) ;
#11678 = ADVANCED_FACE ( 'NONE', ( #4951 ), #3778, .T. ) ;
#11679 = AXIS2_PLACEMENT_3D ( 'NONE', #8289, #7296, #5768 ) ;
#11680 = CARTESIAN_POINT ( 'NONE',  ( 0.04999671152047817368, -2.439987328296867819, -14.75565684666129762 ) ) ;
#11681 = EDGE_CURVE ( 'NONE', #4006, #12755, #11183, .T. ) ;
#11682 = ORIENTED_EDGE ( 'NONE', *, *, #1846, .T. ) ;
#11683 = CARTESIAN_POINT ( 'NONE',  ( 0.000000000000000000, -22.25075486061732732, -9.324097380959701198 ) ) ;
#11684 = ADVANCED_FACE ( 'NONE', ( #310 ), #9855, .F. ) ;
#11685 = VECTOR ( 'NONE', #2315, 1000.000000000000000 ) ;
#11686 = VERTEX_POINT ( 'NONE', #1552 ) ;
#11687 = CARTESIAN_POINT ( 'NONE',  ( 2.031033467310412011, -24.32849926382740335, -12.98167595241049277 ) ) ;
#11688 = DIRECTION ( 'NONE',  ( 0.000000000000000000, 0.000000000000000000, 1.000000000000000000 ) ) ;
#11689 = ORIENTED_EDGE ( 'NONE', *, *, #10755, .T. ) ;
#11690 = ORIENTED_EDGE ( 'NONE', *, *, #8106, .F. ) ;
#11691 = AXIS2_PLACEMENT_3D ( 'NONE', #9156, #11307, #12537 ) ;
#11692 = AXIS2_PLACEMENT_3D ( 'NONE', #12501, #1975, #6659 ) ;
#11693 = EDGE_CURVE ( 'NONE', #14392, #12029, #14399, .T. ) ;
#11694 = CARTESIAN_POINT ( 'NONE',  ( 31.51081190520435626, 3.030430839836910639, 7.000000000000000000 ) ) ;
#11695 = ORIENTED_EDGE ( 'NONE', *, *, #12875, .T. ) ;
#11696 = COLOUR_RGB ( '',0.8941176470588234615, 0.8941176470588234615, 0.8941176470588234615 ) ;
#11697 = CARTESIAN_POINT ( 'NONE',  ( 6.560148031203755073E-16, 23.69843731927177544, -5.456805104200854295 ) ) ;
#11698 = CARTESIAN_POINT ( 'NONE',  ( -3.751931928061364552, 0.6025004624012588739, 7.799999999999990052 ) ) ;
#11699 = CARTESIAN_POINT ( 'NONE',  ( 2.765633920072235519, 18.55949924794892780, 16.37294372382865504 ) ) ;
#11700 = CARTESIAN_POINT ( 'NONE',  ( 1.749999999999999778, -17.29145405592692342, 4.835383649608411716 ) ) ;
#11701 = ADVANCED_FACE ( 'NONE', ( #14553 ), #12148, .F. ) ;
#11702 = AXIS2_PLACEMENT_3D ( 'NONE', #11361, #832, #12587 ) ;
#11703 = ORIENTED_EDGE ( 'NONE', *, *, #3517, .T. ) ;
#11704 = CARTESIAN_POINT ( 'NONE',  ( 0.000000000000000000, 12.98979500319694225, 5.249430348645796940 ) ) ;
#11705 = DIRECTION ( 'NONE',  ( 1.000000000000000000, 0.000000000000000000, 0.000000000000000000 ) ) ;
#11706 = ORIENTED_EDGE ( 'NONE', *, *, #10238, .F. ) ;
#11707 = ADVANCED_FACE ( 'NONE', ( #3947 ), #10782, .F. ) ;
#11708 = B_SPLINE_CURVE_WITH_KNOTS ( 'NONE', 3,
 ( #6667, #10343, #2047, #888 ),
 .UNSPECIFIED., .F., .F.,
 ( 4, 4 ),
 ( 4.462636695653741059E-07, 0.0004963285629696456008 ),
 .UNSPECIFIED. ) ;
#11709 = EDGE_LOOP ( 'NONE', ( #14454, #4875 ) ) ;
#11710 = CARTESIAN_POINT ( 'NONE',  ( 2.030753603471114221, 24.32906614999634698, -12.98165646470055634 ) ) ;
#11711 = CARTESIAN_POINT ( 'NONE',  ( -0.1085714285714285687, -3.798448662927795372, -0.8000000000000000444 ) ) ;
#11712 = EDGE_CURVE ( 'NONE', #2051, #15036, #9702, .T. ) ;
#11713 = ADVANCED_FACE ( 'NONE', ( #6324 ), #9716, .T. ) ;
#11714 = AXIS2_PLACEMENT_3D ( 'NONE', #1800, #9158, #6778 ) ;
#11715 = DIRECTION ( 'NONE',  ( -1.000000000000000000, -0.000000000000000000, -0.000000000000000000 ) ) ;
#11716 = DIRECTION ( 'NONE',  ( -1.000000000000000000, -0.000000000000000000, -0.000000000000000000 ) ) ;
#11717 = ITEM_DEFINED_TRANSFORMATION ( 'NONE', 'NONE', #6716,  #1376 ) ;
#11718 = DIRECTION ( 'NONE',  ( 1.000000000000000000, 0.000000000000000000, 0.000000000000000000 ) ) ;
#11719 = AXIS2_PLACEMENT_3D ( 'NONE', #5757, #1924, #5615 ) ;
#11720 = AXIS2_PLACEMENT_3D ( 'NONE', #6403, #5348, #5261 ) ;
#11721 = DIRECTION ( 'NONE',  ( 0.000000000000000000, 0.000000000000000000, 1.000000000000000000 ) ) ;
#11722 = VERTEX_POINT ( 'NONE', #2640 ) ;
#11723 = LINE ( 'NONE', #4745, #2420 ) ;
#11724 = DIRECTION ( 'NONE',  ( 0.000000000000000000, 0.000000000000000000, 1.000000000000000000 ) ) ;
#11725 = CARTESIAN_POINT ( 'NONE',  ( 1.039999999999996927, -25.12109765559644714, -12.52377138324250438 ) ) ;
#11726 = CARTESIAN_POINT ( 'NONE',  ( 2.030753605846573606, -3.797885586973408056, 27.31305418910209326 ) ) ;
#11727 = ORIENTED_EDGE ( 'NONE', *, *, #12004, .T. ) ;
#11728 = VECTOR ( 'NONE', #3998, 999.9999999999998863 ) ;
#11729 = ADVANCED_FACE ( 'NONE', ( #11082 ), #7334, .T. ) ;
#11730 = ORIENTED_EDGE ( 'NONE', *, *, #6985, .T. ) ;
#11731 = ADVANCED_FACE ( 'NONE', ( #2863 ), #7559, .F. ) ;
#11732 = DIRECTION ( 'NONE',  ( -1.000000000000000000, -0.000000000000000000, -0.000000000000000000 ) ) ;
#11733 = ORIENTED_EDGE ( 'NONE', *, *, #9841, .F. ) ;
#11734 = VECTOR ( 'NONE', #6033, 1000.000000000000114 ) ;
#11735 = AXIS2_PLACEMENT_3D ( 'NONE', #13884, #6742, #819 ) ;
#11736 = CARTESIAN_POINT ( 'NONE',  ( 1.394999999999999574, -12.83329210556822986, -12.55714665600000757 ) ) ;
#11737 = DIRECTION ( 'NONE',  ( -0.9863939238321437486, -0.1643989873053572359, 0.000000000000000000 ) ) ;
#11738 = ADVANCED_FACE ( 'NONE', ( #13237 ), #2717, .F. ) ;
#11739 = CARTESIAN_POINT ( 'NONE',  ( 0.02531912748606228100, 5.229914364928351489, 13.68080036884350292 ) ) ;
#11740 = CARTESIAN_POINT ( 'NONE',  ( -20.63749999999999929, 5.419062086227038392E-16, 4.424999999999999822 ) ) ;
#11741 = CARTESIAN_POINT ( 'NONE',  ( -20.63749999999999574, 0.000000000000000000, 0.000000000000000000 ) ) ;
#11742 = B_SPLINE_CURVE_WITH_KNOTS ( 'NONE', 3,
 ( #8473, #13163, #8559, #12010 ),
 .UNSPECIFIED., .F., .F.,
 ( 4, 4 ),
 ( 2.324263106244728226E-07, 0.0006888201370294799210 ),
 .UNSPECIFIED. ) ;
#11743 = CARTESIAN_POINT ( 'NONE',  ( 0.7589665283900980386, -27.31260702007172725, -3.797536611356600034 ) ) ;
#11744 = LINE ( 'NONE', #14212, #11630 ) ;
#11745 = EDGE_CURVE ( 'NONE', #8704, #5734, #392, .T. ) ;
#11746 = ORIENTED_EDGE ( 'NONE', *, *, #10395, .F. ) ;
#11747 = B_SPLINE_CURVE_WITH_KNOTS ( 'NONE', 3,
 ( #9452, #8530, #2700, #14146, #8302, #2472, #7395, #452 ),
 .UNSPECIFIED., .F., .F.,
 ( 4, 2, 2, 4 ),
 ( 4.663089416196450148E-07, 0.001898630173449458464, 0.002847712105703373645, 0.003796794037957288825 ),
 .UNSPECIFIED. ) ;
#11748 = DIRECTION ( 'NONE',  ( -1.000000000000000000, 0.000000000000000000, -0.000000000000000000 ) ) ;
#11749 =( REPRESENTATION_RELATIONSHIP ('NONE','NONE', #12685, #5737 ) REPRESENTATION_RELATIONSHIP_WITH_TRANSFORMATION ( #11717 )SHAPE_REPRESENTATION_RELATIONSHIP( ) );
#11750 = AXIS2_PLACEMENT_3D ( 'NONE', #13985, #12968, #2372 ) ;
#11751 = AXIS2_PLACEMENT_3D ( 'NONE', #12923, #3482, #8172 ) ;
#11752 = AXIS2_PLACEMENT_3D ( 'NONE', #7740, #9052, #12425 ) ;
#11753 = CARTESIAN_POINT ( 'NONE',  ( 1.039999999999997593, -24.89775460606841051, 12.96210679857778025 ) ) ;
#11754 = ORIENTED_EDGE ( 'NONE', *, *, #10696, .T. ) ;
#11755 = ORIENTED_EDGE ( 'NONE', *, *, #10238, .T. ) ;
#11756 = ORIENTED_EDGE ( 'NONE', *, *, #6899, .T. ) ;
#11757 = EDGE_LOOP ( 'NONE', ( #5021, #7696, #6288, #9664 ) ) ;
#11758 = CARTESIAN_POINT ( 'NONE',  ( 2.789999999999999147, 0.000000000000000000, 0.000000000000000000 ) ) ;
#11759 = DIRECTION ( 'NONE',  ( 0.000000000000000000, 0.000000000000000000, 1.000000000000000000 ) ) ;
#11760 = FACE_BOUND ( 'NONE', #12914, .T. ) ;
#11761 = DIRECTION ( 'NONE',  ( 0.000000000000000000, 0.000000000000000000, 1.000000000000000000 ) ) ;
#11762 = CIRCLE ( 'NONE', #5413, 24.12539914357697413 ) ;
#11763 = CARTESIAN_POINT ( 'NONE',  ( 0.02436607992776064838, 5.391175441198615914, 24.15498966839965078 ) ) ;
#11764 = ORIENTED_EDGE ( 'NONE', *, *, #6970, .T. ) ;
#11765 = CARTESIAN_POINT ( 'NONE',  ( 8.403944755730119454, -10.79473832354794460, 22.47056274847713908 ) ) ;
#11766 = AXIS2_PLACEMENT_3D ( 'NONE', #14979, #12428, #12511 ) ;
#11767 = ORIENTED_EDGE ( 'NONE', *, *, #12293, .F. ) ;
#11768 = FACE_OUTER_BOUND ( 'NONE', #963, .T. ) ;
#11769 = ADVANCED_FACE ( 'NONE', ( #13468 ), #13305, .T. ) ;
#11770 = DIRECTION ( 'NONE',  ( 0.000000000000000000, 0.000000000000000000, 1.000000000000000000 ) ) ;
#11771 = ORIENTED_EDGE ( 'NONE', *, *, #5681, .T. ) ;
#11772 = ORIENTED_EDGE ( 'NONE', *, *, #6764, .T. ) ;
#11773 = DIRECTION ( 'NONE',  ( 0.1305261922200521840, 0.9914448613738103822, -0.000000000000000000 ) ) ;
#11774 = AXIS2_PLACEMENT_3D ( 'NONE', #14338, #13087, #8641 ) ;
#11775 = ORIENTED_EDGE ( 'NONE', *, *, #9872, .T. ) ;
#11776 = CARTESIAN_POINT ( 'NONE',  ( -1.092452291144053154E-14, 14.05347802000169288, 2.096460570596223594 ) ) ;
#11777 = CARTESIAN_POINT ( 'NONE',  ( -1.000000000000000000, -5.408326913195983465, 0.000000000000000000 ) ) ;
#11778 = CARTESIAN_POINT ( 'NONE',  ( 0.07181523211953061425, 10.24584646439538993, 23.19431517146936983 ) ) ;
#11779 = FACE_OUTER_BOUND ( 'NONE', #3254, .T. ) ;
#11780 = ORIENTED_EDGE ( 'NONE', *, *, #13497, .T. ) ;
#11781 = DIRECTION ( 'NONE',  ( 0.000000000000000000, 0.000000000000000000, 1.000000000000000000 ) ) ;
#11782 = CARTESIAN_POINT ( 'NONE',  ( 1.749999999999998002, -20.02152543075331081, -19.67366047555553266 ) ) ;
#11783 = EDGE_LOOP ( 'NONE', ( #11834, #7800, #6422, #382 ) ) ;
#11784 = ORIENTED_EDGE ( 'NONE', *, *, #9551, .T. ) ;
#11785 = CARTESIAN_POINT ( 'NONE',  ( 0.5537796877189846700, -12.52687487503410679, -11.41743294611088189 ) ) ;
#11786 = LINE ( 'NONE', #14101, #14699 ) ;
#11787 = ADVANCED_FACE ( 'NONE', ( #9927 ), #1865, .F. ) ;
#11788 = CARTESIAN_POINT ( 'NONE',  ( 2.021362740937215019, 5.021526291670316056, 16.74220655292939242 ) ) ;
#11789 = CARTESIAN_POINT ( 'NONE',  ( 98.48580539929344013, 0.9022481406819604643, 2.999999999999999112 ) ) ;
#11790 = DIRECTION ( 'NONE',  ( -0.000000000000000000, 0.000000000000000000, 1.000000000000000000 ) ) ;
#11791 = CARTESIAN_POINT ( 'NONE',  ( 0.006974693931642885793, -18.43727551351043203, 16.17543236987982525 ) ) ;
#11792 = ORIENTED_EDGE ( 'NONE', *, *, #8918, .F. ) ;
#11793 = DIRECTION ( 'NONE',  ( -5.480158469902919838E-17, -1.051478716308701618E-16, -1.000000000000000000 ) ) ;
#11794 = CYLINDRICAL_SURFACE ( 'NONE', #1770, 13.19999999999999929 ) ;
#11795 = DIRECTION ( 'NONE',  ( 0.000000000000000000, 0.000000000000000000, -1.000000000000000000 ) ) ;
#11796 = CARTESIAN_POINT ( 'NONE',  ( 0.006931069955679000985, 16.17493693894905959, -18.43696893154741190 ) ) ;
#11797 = ADVANCED_FACE ( 'NONE', ( #6554 ), #7261, .T. ) ;
#11798 = EDGE_CURVE ( 'NONE', #11164, #8896, #6780, .T. ) ;
#11799 = EDGE_CURVE ( 'NONE', #1932, #3376, #8850, .T. ) ;
#11800 = EDGE_LOOP ( 'NONE', ( #1472, #10479, #10356, #793, #4983, #1177 ) ) ;
#11801 = EDGE_LOOP ( 'NONE', ( #3828, #14326, #12979, #13913, #11650, #6569, #5183, #11527 ) ) ;
#11802 = VERTEX_POINT ( 'NONE', #7784 ) ;
#11803 = CARTESIAN_POINT ( 'NONE',  ( 0.02531912748464804769, 9.232963481057765875, 11.36963888406690870 ) ) ;
#11804 = FACE_OUTER_BOUND ( 'NONE', #8367, .T. ) ;
#11805 = DIRECTION ( 'NONE',  ( -1.000000000000000000, -0.000000000000000000, 0.000000000000000000 ) ) ;
#11806 = CARTESIAN_POINT ( 'NONE',  ( 2.508169719062757874, 10.58084377126639630, -12.18203740414256231 ) ) ;
#11807 = CARTESIAN_POINT ( 'NONE',  ( 80.00000000000000000, 3.469446951953614189E-15, -5.750000000000001776 ) ) ;
#11808 = CARTESIAN_POINT ( 'NONE',  ( 70.16198417812034904, 9.730076655429538590, 2.999999999999999112 ) ) ;
#11809 = VERTEX_POINT ( 'NONE', #12387 ) ;
#11810 = LINE ( 'NONE', #7523, #3937 ) ;
#11811 = DIRECTION ( 'NONE',  ( 1.000000000000000000, 0.000000000000000000, 0.000000000000000000 ) ) ;
#11812 = EDGE_CURVE ( 'NONE', #3507, #10221, #710, .T. ) ;
#11813 = EDGE_CURVE ( 'NONE', #13917, #5604, #118, .T. ) ;
#11814 = EDGE_LOOP ( 'NONE', ( #11168, #9038, #4871, #10947 ) ) ;
#11815 = LINE ( 'NONE', #8009, #8539 ) ;
#11816 = CARTESIAN_POINT ( 'NONE',  ( -1.566204647097437563, -6.822536405429463713, -0.8000000000000000444 ) ) ;
#11817 = DIRECTION ( 'NONE',  ( 0.000000000000000000, 0.000000000000000000, 1.000000000000000000 ) ) ;
#11818 = EDGE_CURVE ( 'NONE', #11571, #4492, #12961, .T. ) ;
#11819 = ORIENTED_EDGE ( 'NONE', *, *, #10100, .T. ) ;
#11820 =( NAMED_UNIT ( * ) PLANE_ANGLE_UNIT ( ) SI_UNIT ( $, .RADIAN. ) );
#11821 = ORIENTED_EDGE ( 'NONE', *, *, #1384, .F. ) ;
#11822 = VERTEX_POINT ( 'NONE', #366 ) ;
#11823 = EDGE_LOOP ( 'NONE', ( #4151, #12599, #7364, #13250 ) ) ;
#11824 = DIRECTION ( 'NONE',  ( 0.000000000000000000, 0.000000000000000000, 1.000000000000000000 ) ) ;
#11825 = LINE ( 'NONE', #1465, #5391 ) ;
#11826 = EDGE_CURVE ( 'NONE', #5700, #672, #14082, .T. ) ;
#11827 = AXIS2_PLACEMENT_3D ( 'NONE', #8574, #8491, #8644 ) ;
#11828 = CARTESIAN_POINT ( 'NONE',  ( 2.764680872513933796, 5.229914364928542447, -13.68080036884343009 ) ) ;
#11829 = DIRECTION ( 'NONE',  ( -0.9988110320138940956, -0.04874958797097371510, -0.000000000000000000 ) ) ;
#11830 = CARTESIAN_POINT ( 'NONE',  ( 1.749999999999999778, 12.83329210556831690, 12.55714665599991875 ) ) ;
#11831 = ORIENTED_EDGE ( 'NONE', *, *, #8472, .F. ) ;
#11832 = CARTESIAN_POINT ( 'NONE',  ( 101.4858053992934401, 0.9022481406819604643, 4.000000000000000000 ) ) ;
#11833 = AXIS2_PLACEMENT_3D ( 'NONE', #13343, #202, #4921 ) ;
#11834 = ORIENTED_EDGE ( 'NONE', *, *, #3432, .T. ) ;
#11835 = CARTESIAN_POINT ( 'NONE',  ( 1.749999999999998002, -24.89775460606821866, -12.96210679857815684 ) ) ;
#11836 = DIRECTION ( 'NONE',  ( 1.000000000000000000, 0.000000000000000000, -0.000000000000000000 ) ) ;
#11837 = ORIENTED_EDGE ( 'NONE', *, *, #3073, .F. ) ;
#11838 = ORIENTED_EDGE ( 'NONE', *, *, #4999, .F. ) ;
#11839 = FACE_OUTER_BOUND ( 'NONE', #324, .T. ) ;
#11840 = ORIENTED_EDGE ( 'NONE', *, *, #1558, .F. ) ;
#11841 = DIRECTION ( 'NONE',  ( -1.000000000000000000, 0.000000000000000000, 0.000000000000000000 ) ) ;
#11842 = CARTESIAN_POINT ( 'NONE',  ( 0.000000000000000000, 0.000000000000000000, 0.000000000000000000 ) ) ;
#11843 = CARTESIAN_POINT ( 'NONE',  ( 0.000000000000000000, -7.739906618939614624, -10.88091150984234545 ) ) ;
#11844 = DIRECTION ( 'NONE',  ( -0.000000000000000000, -0.000000000000000000, 1.000000000000000000 ) ) ;
#11845 = ORIENTED_EDGE ( 'NONE', *, *, #11111, .F. ) ;
#11846 = LINE ( 'NONE', #1191, #5833 ) ;
#11847 = ADVANCED_FACE ( 'NONE', ( #5167 ), #6525, .T. ) ;
#11848 = CYLINDRICAL_SURFACE ( 'NONE', #14153, 13.19999999999999929 ) ;
#11849 = VERTEX_POINT ( 'NONE', #9899 ) ;
#11850 = EDGE_LOOP ( 'NONE', ( #14162, #13150, #7673, #15091 ) ) ;
#11851 = ORIENTED_EDGE ( 'NONE', *, *, #13871, .T. ) ;
#11852 = CARTESIAN_POINT ( 'NONE',  ( 0.1882238782932349475, -17.47009390565476750, -19.18368891937510412 ) ) ;
#11853 = DIRECTION ( 'NONE',  ( -1.000000000000000000, -0.000000000000000000, -0.000000000000000000 ) ) ;
#11854 = COLOUR_RGB ( '',0.8941176470588234615, 0.8941176470588234615, 0.8941176470588234615 ) ;
#11855 = DIRECTION ( 'NONE',  ( 0.000000000000000000, -1.374038396813314756E-15, -1.000000000000000000 ) ) ;
#11856 = DIRECTION ( 'NONE',  ( -1.000000000000000000, -0.000000000000000000, -0.000000000000000000 ) ) ;
#11857 = CARTESIAN_POINT ( 'NONE',  ( 8.000000000000000000, 0.000000000000000000, 0.000000000000000000 ) ) ;
#11858 = EDGE_CURVE ( 'NONE', #154, #2812, #7387, .T. ) ;
#11859 = DIRECTION ( 'NONE',  ( -1.000000000000000000, -0.000000000000000000, -0.000000000000000000 ) ) ;
#11860 = CIRCLE ( 'NONE', #2313, 2.999999999999988898 ) ;
#11861 = EDGE_CURVE ( 'NONE', #5744, #389, #7756, .T. ) ;
#11862 = EDGE_LOOP ( 'NONE', ( #5983, #12078, #10748, #6822, #9418, #8845 ) ) ;
#11863 = CARTESIAN_POINT ( 'NONE',  ( 2.718184757033982990, 18.89296398180191616, 16.91181672897740640 ) ) ;
#11864 = FACE_OUTER_BOUND ( 'NONE', #10939, .T. ) ;
#11865 = CARTESIAN_POINT ( 'NONE',  ( 1.749999999999998002, 27.68468304288265358, -4.633866840648635410 ) ) ;
#11866 = CARTESIAN_POINT ( 'NONE',  ( 2.257825467309740208, -3.467596033028475855, 26.83036154824992892 ) ) ;
#11867 = ORIENTED_EDGE ( 'NONE', *, *, #11798, .T. ) ;
#11868 = ADVANCED_FACE ( 'NONE', ( #13357 ), #2762, .T. ) ;
#11869 = B_SPLINE_CURVE_WITH_KNOTS ( 'NONE', 3,
 ( #1790, #9930, #5421, #12390 ),
 .UNSPECIFIED., .F., .F.,
 ( 4, 4 ),
 ( 0.005258214619651976202, 0.005948481662034167325 ),
 .UNSPECIFIED. ) ;
#11870 = ORIENTED_EDGE ( 'NONE', *, *, #10454, .T. ) ;
#11871 = VECTOR ( 'NONE', #12363, 999.9999999999998863 ) ;
#11872 = VECTOR ( 'NONE', #3559, 1000.000000000000114 ) ;
#11873 = ORIENTED_EDGE ( 'NONE', *, *, #14823, .T. ) ;
#11874 = AXIS2_PLACEMENT_3D ( 'NONE', #8028, #9476, #5730 ) ;
#11875 = CARTESIAN_POINT ( 'NONE',  ( 2.789999999999999147, 24.63872515616082737, 2.336989772644355146 ) ) ;
#11876 = CARTESIAN_POINT ( 'NONE',  ( 0.000000000000000000, 0.000000000000000000, 10.00000000000000000 ) ) ;
#11877 = FACE_OUTER_BOUND ( 'NONE', #14967, .T. ) ;
#11878 = CARTESIAN_POINT ( 'NONE',  ( -6.133727067292549495E-14, 11.12234047011202875, -8.842064619038410456 ) ) ;
#11879 = CARTESIAN_POINT ( 'NONE',  ( 14.40394475573011945, -10.79473832354794460, -5.750000000000008882 ) ) ;
#11880 = CARTESIAN_POINT ( 'NONE',  ( 2.010451917295049906, 5.008579424861795637, -16.73367785739752378 ) ) ;
#11881 = EDGE_CURVE ( 'NONE', #3359, #1805, #12122, .T. ) ;
#11882 = EDGE_CURVE ( 'NONE', #1013, #6387, #11122, .T. ) ;
#11883 = VERTEX_POINT ( 'NONE', #2836 ) ;
#11884 = CARTESIAN_POINT ( 'NONE',  ( 0.000000000000000000, 0.000000000000000000, 0.000000000000000000 ) ) ;
#11885 = DIRECTION ( 'NONE',  ( -1.000000000000000000, -0.000000000000000000, -0.000000000000000000 ) ) ;
#11886 = CIRCLE ( 'NONE', #12391, 6.000000000000005329 ) ;
#11887 = VECTOR ( 'NONE', #6472, 1000.000000000000000 ) ;
#11888 = EDGE_LOOP ( 'NONE', ( #11059, #15094, #12417, #8549 ) ) ;
#11889 = DIRECTION ( 'NONE',  ( 1.000000000000000000, 0.000000000000000000, 0.000000000000000000 ) ) ;
#11890 = DIRECTION ( 'NONE',  ( 0.000000000000000000, 0.000000000000000000, -1.000000000000000000 ) ) ;
#11891 = AXIS2_PLACEMENT_3D ( 'NONE', #12364, #767, #11128 ) ;
#11892 = DIRECTION ( 'NONE',  ( 1.000000000000000000, 0.000000000000000000, 0.000000000000000000 ) ) ;
#11893 = ORIENTED_EDGE ( 'NONE', *, *, #80, .T. ) ;
#11894 = EDGE_LOOP ( 'NONE', ( #2745, #2223, #10737, #8968, #2542, #719 ) ) ;
#11895 = ORIENTED_EDGE ( 'NONE', *, *, #10373, .F. ) ;
#11896 = EDGE_LOOP ( 'NONE', ( #639, #6201, #14614, #6277 ) ) ;
#11897 = DIRECTION ( 'NONE',  ( -1.000000000000000000, -0.000000000000000000, 0.000000000000000000 ) ) ;
#11898 = AXIS2_PLACEMENT_3D ( 'NONE', #9805, #2660, #14572 ) ;
#11899 = EDGE_CURVE ( 'NONE', #4314, #10393, #1530, .T. ) ;
#11900 = CARTESIAN_POINT ( 'NONE',  ( 2.604434514863826156, 10.67816411292164958, 23.63475234378986300 ) ) ;
#11901 = CIRCLE ( 'NONE', #7250, 2.999999999999988898 ) ;
#11902 = DIRECTION ( 'NONE',  ( 0.000000000000000000, 0.000000000000000000, 1.000000000000000000 ) ) ;
#11903 = DIRECTION ( 'NONE',  ( 0.000000000000000000, 0.000000000000000000, 1.000000000000000000 ) ) ;
#11904 = EDGE_CURVE ( 'NONE', #7241, #6140, #129, .T. ) ;
#11905 = EDGE_CURVE ( 'NONE', #14639, #1922, #9759, .T. ) ;
#11906 = CARTESIAN_POINT ( 'NONE',  ( 1.039999999999998037, -4.458161950358621617, 17.39253030560839974 ) ) ;
#11907 = ORIENTED_EDGE ( 'NONE', *, *, #12093, .T. ) ;
#11908 = DIRECTION ( 'NONE',  ( 0.000000000000000000, 0.000000000000000000, 1.000000000000000000 ) ) ;
#11909 = AXIS2_PLACEMENT_3D ( 'NONE', #1023, #5717, #12911 ) ;
#11910 = ORIENTED_EDGE ( 'NONE', *, *, #9458, .T. ) ;
#11911 = DIRECTION ( 'NONE',  ( 1.000000000000000000, -5.782411586589355667E-16, 0.000000000000000000 ) ) ;
#11912 = DIRECTION ( 'NONE',  ( -1.000000000000000000, -0.000000000000000000, -0.000000000000000000 ) ) ;
#11913 = EDGE_LOOP ( 'NONE', ( #8270, #12601, #6601, #4744, #14167, #2566, #6145, #5288, #7054, #7417, #8509, #1702, #2322, #3545, #6874, #3549, #11304, #8673, #4564, #10265, #7799, #4931, #13571, #9901, #1462 ) ) ;
#11914 = EDGE_LOOP ( 'NONE', ( #14867, #10955 ) ) ;
#11915 = AXIS2_PLACEMENT_3D ( 'NONE', #3921, #8599, #1690 ) ;
#11916 = MECHANICAL_DESIGN_GEOMETRIC_PRESENTATION_REPRESENTATION (  '', ( #14925 ), #14682 ) ;
#11917 = FACE_OUTER_BOUND ( 'NONE', #7401, .T. ) ;
#11918 = ORIENTED_EDGE ( 'NONE', *, *, #13585, .F. ) ;
#11919 = LINE ( 'NONE', #4953, #74 ) ;
#11920 = CARTESIAN_POINT ( 'NONE',  ( 2.021362756903531288, -17.00993931356758537, -4.022333916463769476 ) ) ;
#11921 = EDGE_CURVE ( 'NONE', #11083, #4547, #12426, .T. ) ;
#11922 = DIRECTION ( 'NONE',  ( 0.000000000000000000, -1.000000000000000000, -3.435095992033282750E-15 ) ) ;
#11923 = AXIS2_PLACEMENT_3D ( 'NONE', #15001, #9078, #7851 ) ;
#11924 = DIRECTION ( 'NONE',  ( -0.04874958797097372204, 0.9988110320138942066, 0.000000000000000000 ) ) ;
#11925 = ORIENTED_EDGE ( 'NONE', *, *, #6331, .T. ) ;
#11926 = CIRCLE ( 'NONE', #649, 24.12539914357697768 ) ;
#11927 = CARTESIAN_POINT ( 'NONE',  ( 2.789999999999999147, 15.04425356660790136, -20.70663861606255196 ) ) ;
#11928 = CARTESIAN_POINT ( 'NONE',  ( 93.63799900313688340, -2.337932895214617890, 2.999999999999999112 ) ) ;
#11929 =( GEOMETRIC_REPRESENTATION_CONTEXT ( 3 ) GLOBAL_UNCERTAINTY_ASSIGNED_CONTEXT ( ( #8848 ) ) GLOBAL_UNIT_ASSIGNED_CONTEXT ( ( #1546, #11450, #3089 ) ) REPRESENTATION_CONTEXT ( 'NONE', 'WORKASPACE' ) );
#11930 = AXIS2_PLACEMENT_3D ( 'NONE', #4435, #7815, #8874 ) ;
#11931 = ORIENTED_EDGE ( 'NONE', *, *, #4513, .F. ) ;
#11932 = CARTESIAN_POINT ( 'NONE',  ( -1.014714340245882228E-14, -13.21889893246979142, 5.211150952915317269 ) ) ;
#11933 = ORIENTED_EDGE ( 'NONE', *, *, #11921, .T. ) ;
#11934 = ORIENTED_EDGE ( 'NONE', *, *, #1939, .F. ) ;
#11935 = FACE_OUTER_BOUND ( 'NONE', #10691, .T. ) ;
#11936 = DIRECTION ( 'NONE',  ( 1.000000000000000000, 0.000000000000000000, 0.000000000000000000 ) ) ;
#11937 = AXIS2_PLACEMENT_3D ( 'NONE', #4221, #14985, #8055 ) ;
#11938 = CARTESIAN_POINT ( 'NONE',  ( 0.000000000000000000, 0.000000000000000000, 4.000000000000000000 ) ) ;
#11939 = CARTESIAN_POINT ( 'NONE',  ( 0.7592463977762118343, 4.828194074574732930, -27.14986936243569460 ) ) ;
#11940 = DIRECTION ( 'NONE',  ( 0.000000000000000000, 0.000000000000000000, 1.000000000000000000 ) ) ;
#11941 = ADVANCED_FACE ( 'NONE', ( #4069 ), #8600, .F. ) ;
#11942 = CIRCLE ( 'NONE', #13668, 28.06981291497571007 ) ;
#11943 = ORIENTED_EDGE ( 'NONE', *, *, #1223, .T. ) ;
#11944 = CARTESIAN_POINT ( 'NONE',  ( 2.715264182578263963, -5.299647274067199376, 14.31752701692935403 ) ) ;
#11945 = DIRECTION ( 'NONE',  ( -1.000000000000000000, 0.000000000000000000, 0.000000000000000000 ) ) ;
#11946 = CARTESIAN_POINT ( 'NONE',  ( 88.46153288930041469, 16.46030115554384565, -2.000000000000000888 ) ) ;
#11947 = CARTESIAN_POINT ( 'NONE',  ( 0.0003207540509381473352, -20.70663861606275447, -12.51925356660783528 ) ) ;
#11948 = ORIENTED_EDGE ( 'NONE', *, *, #11858, .F. ) ;
#11949 = EDGE_LOOP ( 'NONE', ( #3746, #12356, #5046, #2777 ) ) ;
#11950 = EDGE_CURVE ( 'NONE', #2971, #9211, #12286, .T. ) ;
#11951 = ORIENTED_EDGE ( 'NONE', *, *, #5713, .F. ) ;
#11952 = AXIS2_PLACEMENT_3D ( 'NONE', #9189, #6591, #2118 ) ;
#11953 = AXIS2_PLACEMENT_3D ( 'NONE', #4510, #14975, #6734 ) ;
#11954 = CARTESIAN_POINT ( 'NONE',  ( 0.002680699106061737880, 13.26676317347984657, -5.214906618939570748 ) ) ;
#11955 = DIRECTION ( 'NONE',  ( 1.000000000000000000, 0.000000000000000000, 0.000000000000000000 ) ) ;
#11956 = EDGE_CURVE ( 'NONE', #7258, #11060, #8237, .T. ) ;
#11957 = AXIS2_PLACEMENT_3D ( 'NONE', #9092, #13777, #7602 ) ;
#11958 = CARTESIAN_POINT ( 'NONE',  ( 0.7795480827049465766, 5.008579424861561158, 16.73367785739759128 ) ) ;
#11959 = CARTESIAN_POINT ( 'NONE',  ( 2.789999999999999147, -15.74360496233394002, 18.28042085475272671 ) ) ;
#11960 = CARTESIAN_POINT ( 'NONE',  ( 0.000000000000000000, 0.000000000000000000, -5.750000000000001776 ) ) ;
#11961 = CARTESIAN_POINT ( 'NONE',  ( 2.597943565934061283, 5.295083827234923213, -14.93837896275544352 ) ) ;
#11962 = ORIENTED_EDGE ( 'NONE', *, *, #8689, .T. ) ;
#11963 = LINE ( 'NONE', #10968, #10312 ) ;
#11964 = CARTESIAN_POINT ( 'NONE',  ( 0.000000000000000000, 18.28042085475300382, -15.74360496233363804 ) ) ;
#11965 = VERTEX_POINT ( 'NONE', #13213 ) ;
#11966 = DIRECTION ( 'NONE',  ( -0.000000000000000000, 1.000000000000000000, 1.224646799147353207E-16 ) ) ;
#11967 = DIRECTION ( 'NONE',  ( -0.4036950204470283188, 0.9148936170212761398, 0.000000000000000000 ) ) ;
#11968 = AXIS2_PLACEMENT_3D ( 'NONE', #1335, #6032, #9404 ) ;
#11969 = DIRECTION ( 'NONE',  ( -1.000000000000000000, -0.000000000000000000, 0.000000000000000000 ) ) ;
#11970 = ORIENTED_EDGE ( 'NONE', *, *, #5060, .T. ) ;
#11971 = CIRCLE ( 'NONE', #4887, 5.999999999999999112 ) ;
#11972 = CARTESIAN_POINT ( 'NONE',  ( 2.236220346785067647, 16.55730827443872855, -3.624349476775184709 ) ) ;
#11973 = EDGE_LOOP ( 'NONE', ( #223, #1650, #15035, #775 ) ) ;
#11974 = ORIENTED_EDGE ( 'NONE', *, *, #11336, .F. ) ;
#11975 = VERTEX_POINT ( 'NONE', #13521 ) ;
#11976 = DIRECTION ( 'NONE',  ( 1.000000000000000000, 0.000000000000000000, 0.000000000000000000 ) ) ;
#11977 = DIRECTION ( 'NONE',  ( 1.000000000000000000, 0.000000000000000000, 0.000000000000000000 ) ) ;
#11978 = CLOSED_SHELL ( 'NONE', ( #3275, #6572, #6079, #650, #2113, #6612, #13785, #7773, #2620, #12301, #7228, #5248, #9735, #11738, #10481, #12829, #6006, #3563, #11237, #11664, #3732, #3252, #10589, #9770, #10092, #725, #11547, #6021, #532, #1722, #1882, #1809, #10341, #2703 ) ) ;
#11979 = DIRECTION ( 'NONE',  ( -1.000000000000000000, -0.000000000000000000, -0.000000000000000000 ) ) ;
#11980 = CARTESIAN_POINT ( 'NONE',  ( 0.006931069955678739909, -16.17493693894892104, 18.43696893154752914 ) ) ;
#11981 = CARTESIAN_POINT ( 'NONE',  ( 93.34550147531103903, 3.654933296868752457, 6.000000000000000000 ) ) ;
#11982 = ADVANCED_FACE ( 'NONE', ( #8521 ), #2989, .T. ) ;
#11983 = CARTESIAN_POINT ( 'NONE',  ( 2.236220312281012035, 11.41743294611075399, 12.52687487503423291 ) ) ;
#11984 = AXIS2_PLACEMENT_3D ( 'NONE', #5859, #11977, #6151 ) ;
#11985 = CIRCLE ( 'NONE', #5392, 3.799999999999998934 ) ;
#11986 = VERTEX_POINT ( 'NONE', #12519 ) ;
#11987 = CARTESIAN_POINT ( 'NONE',  ( 2.789999999999999147, 15.04425356660790136, -20.70663861606255196 ) ) ;
#11988 = B_SPLINE_CURVE_WITH_KNOTS ( 'NONE', 3,
 ( #6378, #450, #12127, #12359, #6303, #1618 ),
 .UNSPECIFIED., .F., .F.,
 ( 4, 2, 4 ),
 ( 0.0004963285629696456008, 0.002127826186449799806, 0.003759323809929954012 ),
 .UNSPECIFIED. ) ;
#11989 = EDGE_CURVE ( 'NONE', #4328, #15073, #9674, .T. ) ;
#11990 = EDGE_CURVE ( 'NONE', #5125, #12375, #11288, .T. ) ;
#11991 = ORIENTED_EDGE ( 'NONE', *, *, #12045, .T. ) ;
#11992 = ORIENTED_EDGE ( 'NONE', *, *, #13229, .F. ) ;
#11993 = AXIS2_PLACEMENT_3D ( 'NONE', #815, #5522, #7898 ) ;
#11994 = FACE_OUTER_BOUND ( 'NONE', #10819, .T. ) ;
#11995 = DIRECTION ( 'NONE',  ( 0.000000000000000000, 0.000000000000000000, 1.000000000000000000 ) ) ;
#11996 = ORIENTED_EDGE ( 'NONE', *, *, #8169, .T. ) ;
#11997 = VERTEX_POINT ( 'NONE', #7908 ) ;
#11998 = DIRECTION ( 'NONE',  ( 0.000000000000000000, 0.000000000000000000, -1.000000000000000000 ) ) ;
#11999 = ORIENTED_EDGE ( 'NONE', *, *, #842, .F. ) ;
#12000 = DIRECTION ( 'NONE',  ( 0.000000000000000000, 0.000000000000000000, 1.000000000000000000 ) ) ;
#12001 = CYLINDRICAL_SURFACE ( 'NONE', #7591, 4.000000000000000000 ) ;
#12002 = EDGE_CURVE ( 'NONE', #11083, #14739, #1626, .T. ) ;
#12003 = AXIS2_PLACEMENT_3D ( 'NONE', #2704, #9909, #10994 ) ;
#12004 = EDGE_CURVE ( 'NONE', #9979, #10618, #7978, .T. ) ;
#12005 = DIRECTION ( 'NONE',  ( -0.000000000000000000, -0.000000000000000000, 1.000000000000000000 ) ) ;
#12006 = CARTESIAN_POINT ( 'NONE',  ( 1.749999999999998002, -27.68468304288255766, -4.633866840649213614 ) ) ;
#12007 = VERTEX_POINT ( 'NONE', #13748 ) ;
#12008 = CARTESIAN_POINT ( 'NONE',  ( 0.02436607992775978102, 2.336989772644613161, -24.63872515616080250 ) ) ;
#12009 = EDGE_CURVE ( 'NONE', #1997, #85, #1627, .T. ) ;
#12010 = CARTESIAN_POINT ( 'NONE',  ( 2.789999999999999147, -18.28042085475266276, -15.74360496233401996 ) ) ;
#12011 = ORIENTED_EDGE ( 'NONE', *, *, #8072, .F. ) ;
#12012 = CARTESIAN_POINT ( 'NONE',  ( 2.765633920072239516, -24.63872515616084513, 2.336989772644183283 ) ) ;
#12013 = FACE_OUTER_BOUND ( 'NONE', #5188, .T. ) ;
#12014 = VERTEX_POINT ( 'NONE', #3150 ) ;
#12015 = ORIENTED_EDGE ( 'NONE', *, *, #1543, .T. ) ;
#12016 = PRESENTATION_STYLE_ASSIGNMENT (( #14331 ) ) ;
#12017 = CIRCLE ( 'NONE', #741, 24.12539914357697413 ) ;
#12018 = CARTESIAN_POINT ( 'NONE',  ( 1.039999999999996483, -12.55714665599978375, -12.83329210556844835 ) ) ;
#12019 = EDGE_CURVE ( 'NONE', #7858, #2455, #828, .T. ) ;
#12020 = DIRECTION ( 'NONE',  ( 0.000000000000000000, 0.000000000000000000, 1.000000000000000000 ) ) ;
#12021 = CARTESIAN_POINT ( 'NONE',  ( 0.02436607992776455150, 5.391175441198956086, -24.15498966839956907 ) ) ;
#12022 = LINE ( 'NONE', #8849, #11015 ) ;
#12023 = CARTESIAN_POINT ( 'NONE',  ( 101.6227766016837819, 5.204170427930421283E-15, 6.000000000000005329 ) ) ;
#12024 = ORIENTED_EDGE ( 'NONE', *, *, #12546, .F. ) ;
#12025 = CARTESIAN_POINT ( 'NONE',  ( 31.51081190520435626, 3.030430839836910639, -2.000000000000000888 ) ) ;
#12026 = DIRECTION ( 'NONE',  ( -0.000000000000000000, -0.000000000000000000, -1.000000000000000000 ) ) ;
#12027 = CYLINDRICAL_SURFACE ( 'NONE', #9793, 2.524999999999995914 ) ;
#12028 = EDGE_LOOP ( 'NONE', ( #3171, #11669, #7366, #8944 ) ) ;
#12029 = VERTEX_POINT ( 'NONE', #12655 ) ;
#12030 = ORIENTED_EDGE ( 'NONE', *, *, #5919, .T. ) ;
#12031 = CARTESIAN_POINT ( 'NONE',  ( 79.18363542992865689, -10.13606076167855541, 7.000000000000006217 ) ) ;
#12032 = CARTESIAN_POINT ( 'NONE',  ( 13.28797974610714761, -21.11867004231547540, 4.000000000000003553 ) ) ;
#12033 = B_SPLINE_CURVE_WITH_KNOTS ( 'NONE', 3,
 ( #12729, #13813, #10204, #2055 ),
 .UNSPECIFIED., .F., .F.,
 ( 4, 4 ),
 ( 0.005123742438166215690, 0.005814376014856852300 ),
 .UNSPECIFIED. ) ;
#12034 = DIRECTION ( 'NONE',  ( 0.000000000000000000, -0.5877852522924743583, 0.8090169943749465631 ) ) ;
#12035 = CARTESIAN_POINT ( 'NONE',  ( 2.783025306068355853, -16.17543236988001354, 18.43727551351025795 ) ) ;
#12036 = CARTESIAN_POINT ( 'NONE',  ( 2.236220367026668931, 5.139875429512081872, -16.15122426806984279 ) ) ;
#12037 = VERTEX_POINT ( 'NONE', #5534 ) ;
#12038 = CARTESIAN_POINT ( 'NONE',  ( 50.00050000000000239, 4.898587196589412829E-16, -4.000000000000000000 ) ) ;
#12039 = CARTESIAN_POINT ( 'NONE',  ( 80.00000000000000000, 0.000000000000000000, -130.1575142076926852 ) ) ;
#12040 = ORIENTED_EDGE ( 'NONE', *, *, #7849, .F. ) ;
#12041 = CYLINDRICAL_SURFACE ( 'NONE', #6095, 7.000000000000000000 ) ;
#12042 = CARTESIAN_POINT ( 'NONE',  ( 1.960886852992457241, 24.44424927289185945, 12.96989951879416125 ) ) ;
#12043 = B_SPLINE_CURVE_WITH_KNOTS ( 'NONE', 3,
 ( #11112, #1676, #12341, #8653, #14584, #7371 ),
 .UNSPECIFIED., .F., .F.,
 ( 4, 2, 4 ),
 ( 4.462636882155291330E-07, 0.001879885203074804561, 0.003759324142461393896 ),
 .UNSPECIFIED. ) ;
#12044 = CARTESIAN_POINT ( 'NONE',  ( 1.039999999999996039, 24.89775460606832169, 12.96210679857795256 ) ) ;
#12045 = EDGE_CURVE ( 'NONE', #4786, #3966, #6390, .T. ) ;
#12046 = ORIENTED_EDGE ( 'NONE', *, *, #7128, .F. ) ;
#12047 = CARTESIAN_POINT ( 'NONE',  ( 0.000000000000000000, 15.04425356660790136, -20.70663861606255196 ) ) ;
#12048 = DIRECTION ( 'NONE',  ( 0.000000000000000000, 0.000000000000000000, 1.000000000000000000 ) ) ;
#12049 = EDGE_LOOP ( 'NONE', ( #10549, #9750, #9311, #7753, #7495, #2384 ) ) ;
#12050 = VERTEX_POINT ( 'NONE', #4524 ) ;
#12051 = ORIENTED_EDGE ( 'NONE', *, *, #12743, .F. ) ;
#12052 = FACE_OUTER_BOUND ( 'NONE', #8989, .T. ) ;
#12053 = CARTESIAN_POINT ( 'NONE',  ( -8.731825252408779477E-15, -11.12243880662607332, -8.842327429719214038 ) ) ;
#12054 = CARTESIAN_POINT ( 'NONE',  ( 0.000000000000000000, 0.000000000000000000, 7.000000000000000000 ) ) ;
#12055 = CARTESIAN_POINT ( 'NONE',  ( 8.000000000000000000, 0.000000000000000000, 0.000000000000000000 ) ) ;
#12056 = DIRECTION ( 'NONE',  ( 1.000000000000000000, 0.000000000000000000, 0.000000000000000000 ) ) ;
#12057 = CARTESIAN_POINT ( 'NONE',  ( 2.789999999999999147, 24.15498966839970052, -5.391175441198366336 ) ) ;
#12058 = ORIENTED_EDGE ( 'NONE', *, *, #6765, .F. ) ;
#12059 = CARTESIAN_POINT ( 'NONE',  ( 0.000000000000000000, -1.991882183130148087, -24.04302995059968140 ) ) ;
#12060 = EDGE_CURVE ( 'NONE', #7147, #9373, #9210, .T. ) ;
#12061 = EDGE_CURVE ( 'NONE', #13607, #7326, #4732, .T. ) ;
#12062 = B_SPLINE_CURVE_WITH_KNOTS ( 'NONE', 3,
 ( #9259, #2262, #2106, #12778 ),
 .UNSPECIFIED., .F., .F.,
 ( 4, 4 ),
 ( 0.005123695899043904586, 0.005814329666474872711 ),
 .UNSPECIFIED. ) ;
#12063 = VERTEX_POINT ( 'NONE', #6901 ) ;
#12064 = ORIENTED_EDGE ( 'NONE', *, *, #10617, .T. ) ;
#12065 = LINE ( 'NONE', #2779, #4561 ) ;
#12066 = CARTESIAN_POINT ( 'NONE',  ( 2.789999999999999147, 25.59481291497571220, 0.000000000000000000 ) ) ;
#12067 = ORIENTED_EDGE ( 'NONE', *, *, #13814, .F. ) ;
#12068 = UNCERTAINTY_MEASURE_WITH_UNIT (LENGTH_MEASURE( 1.000000000000000082E-05 ), #12555, 'distance_accuracy_value', 'NONE');
#12069 = CARTESIAN_POINT ( 'NONE',  ( 1.387778780781445676E-14, 0.000000000000000000, -7.000000000000007994 ) ) ;
#12070 = PRODUCT_DEFINITION ( 'UNKNOWN', '', #2057, #2716 ) ;
#12071 = ADVANCED_FACE ( 'NONE', ( #3224, #1918 ), #11507, .T. ) ;
#12072 = ORIENTED_EDGE ( 'NONE', *, *, #14154, .T. ) ;
#12073 = VECTOR ( 'NONE', #2823, 1000.000000000000000 ) ;
#12074 = EDGE_CURVE ( 'NONE', #15169, #10516, #2859, .T. ) ;
#12075 = CARTESIAN_POINT ( 'NONE',  ( 1.394999999999998685, 12.83329210556831690, 12.55714665599991875 ) ) ;
#12076 = DIRECTION ( 'NONE',  ( 1.000000000000000000, 0.000000000000000000, 0.000000000000000000 ) ) ;
#12077 = DIRECTION ( 'NONE',  ( -1.000000000000000000, -0.000000000000000000, 0.000000000000000000 ) ) ;
#12078 = ORIENTED_EDGE ( 'NONE', *, *, #1667, .F. ) ;
#12079 = FACE_OUTER_BOUND ( 'NONE', #13688, .T. ) ;
#12080 = CARTESIAN_POINT ( 'NONE',  ( 33.82574562093736859, -6.697933970950280091, 4.000000000000000000 ) ) ;
#12081 = VERTEX_POINT ( 'NONE', #3369 ) ;
#12082 = CARTESIAN_POINT ( 'NONE',  ( 6.000000000000000888, 0.000000000000000000, 4.500000000000000888 ) ) ;
#12083 = LINE ( 'NONE', #1138, #4541 ) ;
#12084 = AXIS2_PLACEMENT_3D ( 'NONE', #7415, #13072, #2561 ) ;
#12085 = B_SPLINE_CURVE_WITH_KNOTS ( 'NONE', 3,
 ( #1825, #3481, #1106, #9334, #12704, #5384, #7018, #2261 ),
 .UNSPECIFIED., .F., .F.,
 ( 4, 2, 2, 4 ),
 ( 4.663089340421306733E-07, 0.001898630032275575984, 0.002847711893946347668, 0.003796793755617119785 ),
 .UNSPECIFIED. ) ;
#12086 = ORIENTED_EDGE ( 'NONE', *, *, #4695, .F. ) ;
#12087 = ORIENTED_EDGE ( 'NONE', *, *, #8691, .T. ) ;
#12088 = CARTESIAN_POINT ( 'NONE',  ( 76.00000000000000000, 4.898587196589422689E-16, 4.000000000000003553 ) ) ;
#12089 = CARTESIAN_POINT ( 'NONE',  ( 2.262072769566604080, -11.57956866523201178, -24.43806413951687873 ) ) ;
#12090 = ADVANCED_FACE ( 'NONE', ( #8058 ), #4226, .T. ) ;
#12091 = PLANE ( 'NONE',  #12928 ) ;
#12092 = PLANE ( 'NONE',  #10924 ) ;
#12093 = EDGE_CURVE ( 'NONE', #448, #3664, #13587, .T. ) ;
#12094 = CYLINDRICAL_SURFACE ( 'NONE', #12494, 13.19999999999999929 ) ;
#12095 = ORIENTED_EDGE ( 'NONE', *, *, #10416, .T. ) ;
#12096 = CARTESIAN_POINT ( 'NONE',  ( 2.789999999999999147, 15.74360496233381390, 18.28042085475283685 ) ) ;
#12097 = DIRECTION ( 'NONE',  ( -0.9863939238321437486, -0.1643989873053574857, 0.000000000000000000 ) ) ;
#12098 = LINE ( 'NONE', #11034, #5639 ) ;
#12099 = DIRECTION ( 'NONE',  ( 0.000000000000000000, 0.000000000000000000, 1.000000000000000000 ) ) ;
#12100 = ADVANCED_FACE ( 'NONE', ( #5462 ), #637, .T. ) ;
#12101 = EDGE_LOOP ( 'NONE', ( #2027, #14391, #11893, #9678, #8736, #880, #1022, #14762 ) ) ;
#12102 = ORIENTED_EDGE ( 'NONE', *, *, #4419, .F. ) ;
#12103 = CARTESIAN_POINT ( 'NONE',  ( 2.790000000000011138, 13.21889893246973813, 5.211150952915412304 ) ) ;
#12104 = VERTEX_POINT ( 'NONE', #13356 ) ;
#12105 = DIRECTION ( 'NONE',  ( 1.000000000000000000, 0.000000000000000000, 0.000000000000000000 ) ) ;
#12106 = LINE ( 'NONE', #7369, #6322 ) ;
#12107 = FACE_OUTER_BOUND ( 'NONE', #10669, .T. ) ;
#12108 = CARTESIAN_POINT ( 'NONE',  ( -14.40394475573012301, -16.79473832354794993, 20.00000000000000000 ) ) ;
#12109 = DIRECTION ( 'NONE',  ( 0.000000000000000000, 0.000000000000000000, 1.000000000000000000 ) ) ;
#12110 = CARTESIAN_POINT ( 'NONE',  ( 98.63205416320636232, -2.094184955359748468, 4.000000000000000000 ) ) ;
#12111 = ORIENTED_EDGE ( 'NONE', *, *, #6239, .T. ) ;
#12112 = LINE ( 'NONE', #6138, #12988 ) ;
#12113 = CARTESIAN_POINT ( 'NONE',  ( 2.789999999999999147, 0.000000000000000000, 0.000000000000000000 ) ) ;
#12114 = VERTEX_POINT ( 'NONE', #5085 ) ;
#12115 = LINE ( 'NONE', #2688, #5372 ) ;
#12116 = CARTESIAN_POINT ( 'NONE',  ( 1.149999999999998135, 4.959819536546779614E-16, 4.000000000000000000 ) ) ;
#12117 = CARTESIAN_POINT ( 'NONE',  ( 2.257825477245766432, -18.57583492944434411, 19.66801664102697345 ) ) ;
#12118 = VERTEX_POINT ( 'NONE', #8663 ) ;
#12119 = CIRCLE ( 'NONE', #5517, 6.000000000000000000 ) ;
#12120 = AXIS2_PLACEMENT_3D ( 'NONE', #9309, #999, #15003 ) ;
#12121 = CARTESIAN_POINT ( 'NONE',  ( 2.715264205769559958, 15.04916547791930270, -2.569134216958818495 ) ) ;
#12122 = LINE ( 'NONE', #6374, #5072 ) ;
#12123 = VERTEX_POINT ( 'NONE', #8520 ) ;
#12124 = ORIENTED_EDGE ( 'NONE', *, *, #8427, .T. ) ;
#12125 = ORIENTED_EDGE ( 'NONE', *, *, #13612, .T. ) ;
#12126 = CARTESIAN_POINT ( 'NONE',  ( 2.789999999999999147, 24.04302995059966364, -1.991882183130384121 ) ) ;
#12127 = CARTESIAN_POINT ( 'NONE',  ( 0.4314184204727332661, 23.43037373958377501, 12.94152279942384709 ) ) ;
#12128 = DIRECTION ( 'NONE',  ( -0.000000000000000000, -0.000000000000000000, -1.000000000000000000 ) ) ;
#12129 = LINE ( 'NONE', #4232, #11871 ) ;
#12130 = DIRECTION ( 'NONE',  ( -0.9873505073845697533, 0.1585527532634883052, 0.000000000000000000 ) ) ;
#12131 = AXIS2_PLACEMENT_3D ( 'NONE', #9843, #5240, #3931 ) ;
#12132 = AXIS2_PLACEMENT_3D ( 'NONE', #2642, #10853, #312 ) ;
#12133 = AXIS2_PLACEMENT_3D ( 'NONE', #12956, #11732, #8273 ) ;
#12134 = DIRECTION ( 'NONE',  ( 0.000000000000000000, 0.000000000000000000, 1.000000000000000000 ) ) ;
#12135 = EDGE_CURVE ( 'NONE', #1922, #12657, #4191, .T. ) ;
#12136 = ORIENTED_EDGE ( 'NONE', *, *, #7015, .T. ) ;
#12137 = CARTESIAN_POINT ( 'NONE',  ( 2.790000000000000924, 0.000000000000000000, 0.000000000000000000 ) ) ;
#12138 = AXIS2_PLACEMENT_3D ( 'NONE', #11879, #14281, #7205 ) ;
#12139 = AXIS2_PLACEMENT_3D ( 'NONE', #2905, #3907, #5381 ) ;
#12140 = TOROIDAL_SURFACE ( 'NONE', #5307, 24.12539914357697768, 8.000000000000000000 ) ;
#12141 = VERTEX_POINT ( 'NONE', #7386 ) ;
#12142 = ORIENTED_EDGE ( 'NONE', *, *, #6158, .F. ) ;
#12143 = CARTESIAN_POINT ( 'NONE',  ( 2.789999999999999147, -11.04103753892265694, -8.624777288397918795 ) ) ;
#12144 = EDGE_CURVE ( 'NONE', #6030, #13716, #13345, .T. ) ;
#12145 = CARTESIAN_POINT ( 'NONE',  ( 2.789999999999999147, -13.87420763704359850, -1.948757464274317508 ) ) ;
#12146 = ORIENTED_EDGE ( 'NONE', *, *, #10787, .F. ) ;
#12147 = EDGE_CURVE ( 'NONE', #10776, #8684, #5005, .T. ) ;
#12148 = CYLINDRICAL_SURFACE ( 'NONE', #14630, 4.999999999999997335 ) ;
#12149 = CIRCLE ( 'NONE', #9457, 4.000000000000003553 ) ;
#12150 = VERTEX_POINT ( 'NONE', #6373 ) ;
#12151 = AXIS2_PLACEMENT_3D ( 'NONE', #14393, #14706, #1781 ) ;
#12152 = LINE ( 'NONE', #11314, #13366 ) ;
#12153 = ADVANCED_FACE ( 'NONE', ( #2761 ), #9834, .F. ) ;
#12154 = FACE_OUTER_BOUND ( 'NONE', #5749, .T. ) ;
#12155 = LINE ( 'NONE', #5196, #13601 ) ;
#12156 = CARTESIAN_POINT ( 'NONE',  ( 0.1085714285714285687, -3.798448662927795372, -0.8000000000000000444 ) ) ;
#12157 = CARTESIAN_POINT ( 'NONE',  ( 93.63799900313688340, -2.337932895214617890, 2.999999999999999112 ) ) ;
#12158 = ORIENTED_EDGE ( 'NONE', *, *, #344, .F. ) ;
#12159 = DIRECTION ( 'NONE',  ( 0.02857142857142857401, -0.9995917534020515305, 0.000000000000000000 ) ) ;
#12160 = AXIS2_PLACEMENT_3D ( 'NONE', #7677, #5006, #5683 ) ;
#12161 = EDGE_CURVE ( 'NONE', #447, #13730, #4337, .T. ) ;
#12162 = DIRECTION ( 'NONE',  ( 1.000000000000000000, -0.000000000000000000, 0.000000000000000000 ) ) ;
#12163 = VERTEX_POINT ( 'NONE', #2920 ) ;
#12164 = ORIENTED_EDGE ( 'NONE', *, *, #14027, .F. ) ;
#12165 = LINE ( 'NONE', #2171, #9031 ) ;
#12166 = DIRECTION ( 'NONE',  ( 0.000000000000000000, 0.000000000000000000, 1.000000000000000000 ) ) ;
#12167 = B_SPLINE_CURVE_WITH_KNOTS ( 'NONE', 3,
 ( #6248, #14491, #3871, #8468, #8553, #7339 ),
 .UNSPECIFIED., .F., .F.,
 ( 4, 2, 4 ),
 ( 4.462636695653741059E-07, 0.001879885036799761131, 0.003759323809929956614 ),
 .UNSPECIFIED. ) ;
#12168 = CARTESIAN_POINT ( 'NONE',  ( 86.00000000000000000, 0.000000000000000000, 4.500000000000000888 ) ) ;
#12169 = AXIS2_PLACEMENT_3D ( 'NONE', #10895, #13205, #3986 ) ;
#12170 = EDGE_CURVE ( 'NONE', #910, #7573, #9971, .T. ) ;
#12171 = FACE_OUTER_BOUND ( 'NONE', #2922, .T. ) ;
#12172 = AXIS2_PLACEMENT_3D ( 'NONE', #13816, #4454, #9134 ) ;
#12173 = ORIENTED_EDGE ( 'NONE', *, *, #1854, .T. ) ;
#12174 = DIRECTION ( 'NONE',  ( -1.000000000000000000, 0.000000000000000000, 0.000000000000000000 ) ) ;
#12175 = CARTESIAN_POINT ( 'NONE',  ( -9.999999999999998224, 0.000000000000000000, 4.000000000000003553 ) ) ;
#12176 = COLOUR_RGB ( '',1.000000000000000000, 0.9490196078431372140, 0.9098039215686274384 ) ;
#12177 = AXIS2_PLACEMENT_3D ( 'NONE', #13729, #3042, #11334 ) ;
#12178 = DIRECTION ( 'NONE',  ( -0.000000000000000000, -0.000000000000000000, 1.000000000000000000 ) ) ;
#12179 = B_SPLINE_CURVE_WITH_KNOTS ( 'NONE', 3,
 ( #8980, #3227, #15057, #8062, #3155, #12737 ),
 .UNSPECIFIED., .F., .F.,
 ( 4, 2, 4 ),
 ( 2.586195665736120714E-07, 0.001878649493629689022, 0.003757040367692804708 ),
 .UNSPECIFIED. ) ;
#12180 = DIRECTION ( 'NONE',  ( 0.000000000000000000, 0.000000000000000000, -1.000000000000000000 ) ) ;
#12181 = EDGE_CURVE ( 'NONE', #10971, #12986, #9981, .T. ) ;
#12182 = ORIENTED_EDGE ( 'NONE', *, *, #1259, .F. ) ;
#12183 = VERTEX_POINT ( 'NONE', #514 ) ;
#12184 = EDGE_CURVE ( 'NONE', #12375, #2475, #1529, .T. ) ;
#12185 = EDGE_CURVE ( 'NONE', #7731, #1772, #13152, .T. ) ;
#12186 = CIRCLE ( 'NONE', #12435, 4.872650870659752442 ) ;
#12187 = CIRCLE ( 'NONE', #13158, 4.999999999999997335 ) ;
#12188 = VERTEX_POINT ( 'NONE', #4153 ) ;
#12189 = DIRECTION ( 'NONE',  ( -1.000000000000000000, 0.000000000000000000, 0.000000000000000000 ) ) ;
#12190 = CARTESIAN_POINT ( 'NONE',  ( 0.02436607992776064838, 5.391175441198615914, 24.15498966839965078 ) ) ;
#12191 = CIRCLE ( 'NONE', #13164, 4.000000000000000888 ) ;
#12192 = CYLINDRICAL_SURFACE ( 'NONE', #15168, 4.000000000000000000 ) ;
#12193 = DIRECTION ( 'NONE',  ( -1.000000000000000000, 0.000000000000000000, 0.000000000000000000 ) ) ;
#12194 = VECTOR ( 'NONE', #12271, 1000.000000000000000 ) ;
#12195 = CARTESIAN_POINT ( 'NONE',  ( -2.321707774797442170, -4.824281976789052351, 0.000000000000000000 ) ) ;
#12196 = CARTESIAN_POINT ( 'NONE',  ( -10.00000000000000000, 0.000000000000000000, 0.000000000000000000 ) ) ;
#12197 = CARTESIAN_POINT ( 'NONE',  ( 2.789999999999999147, 12.52067188844351442, 20.62201879784917935 ) ) ;
#12198 = EDGE_LOOP ( 'NONE', ( #2303, #1879, #1548, #4373, #5952, #7689 ) ) ;
#12200 = AXIS2_PLACEMENT_3D ( 'NONE', #5887, #1111, #14021 ) ;
#12199 = DIRECTION ( 'NONE',  ( -0.000000000000000000, -0.000000000000000000, -1.000000000000000000 ) ) ;
#12201 = CARTESIAN_POINT ( 'NONE',  ( 1.749999999999998002, 0.000000000000000000, 0.000000000000000000 ) ) ;
#12202 = EDGE_CURVE ( 'NONE', #2590, #12183, #9898, .T. ) ;
#12203 = CARTESIAN_POINT ( 'NONE',  ( 0.007327513813774889397, -5.204526028255783920, 13.44898112152236891 ) ) ;
#12204 = EDGE_CURVE ( 'NONE', #5435, #12653, #5809, .T. ) ;
#12205 = ORIENTED_EDGE ( 'NONE', *, *, #11030, .F. ) ;
#12206 = AXIS2_PLACEMENT_3D ( 'NONE', #8811, #14354, #2972 ) ;
#12207 =( GEOMETRIC_REPRESENTATION_CONTEXT ( 3 ) GLOBAL_UNCERTAINTY_ASSIGNED_CONTEXT ( ( #12068 ) ) GLOBAL_UNIT_ASSIGNED_CONTEXT ( ( #12555, #6793, #1802 ) ) REPRESENTATION_CONTEXT ( 'NONE', 'WORKASPACE' ) );
#12208 = EDGE_CURVE ( 'NONE', #8463, #3989, #6444, .T. ) ;
#12209 = CARTESIAN_POINT ( 'NONE',  ( 2.010451919658913678, 16.99607982911238224, -4.029281904976652839 ) ) ;
#12211 = AXIS2_PLACEMENT_3D ( 'NONE', #7982, #1063, #4530 ) ;
#12210 = DIRECTION ( 'NONE',  ( 0.000000000000000000, 0.000000000000000000, -1.000000000000000000 ) ) ;
#12212 = ORIENTED_EDGE ( 'NONE', *, *, #8243, .F. ) ;
#12213 = VECTOR ( 'NONE', #7100, 1000.000000000000000 ) ;
#12214 = ORIENTED_EDGE ( 'NONE', *, *, #7511, .T. ) ;
#12215 = CARTESIAN_POINT ( 'NONE',  ( 4.271534284832219323E-17, 3.369532131271296443E-15, 6.999999999999989342 ) ) ;
#12216 = DIRECTION ( 'NONE',  ( -1.000000000000000000, 0.000000000000000000, 0.000000000000000000 ) ) ;
#12217 = LINE ( 'NONE', #11214, #11728 ) ;
#12218 = CARTESIAN_POINT ( 'NONE',  ( -5.209999999999999964, 0.000000000000000000, 0.000000000000000000 ) ) ;
#12219 = CARTESIAN_POINT ( 'NONE',  ( 80.00000000000000000, 0.000000000000000000, 7.000000000000000000 ) ) ;
#12220 = EDGE_CURVE ( 'NONE', #6696, #13039, #5311, .T. ) ;
#12221 = AXIS2_PLACEMENT_3D ( 'NONE', #12054, #1, #1385 ) ;
#12222 = CARTESIAN_POINT ( 'NONE',  ( 2.715264245299034762, 9.749517823374011627, 11.74839219818091607 ) ) ;
#12223 = ORIENTED_EDGE ( 'NONE', *, *, #9550, .T. ) ;
#12224 = VECTOR ( 'NONE', #5668, 1000.000000000000000 ) ;
#12225 = CARTESIAN_POINT ( 'NONE',  ( 2.783025325906566927, -2.249040938978666748, 24.42374957165204563 ) ) ;
#12226 = ORIENTED_EDGE ( 'NONE', *, *, #8873, .F. ) ;
#12227 = ORIENTED_EDGE ( 'NONE', *, *, #3929, .F. ) ;
#12228 = ORIENTED_EDGE ( 'NONE', *, *, #15214, .F. ) ;
#12229 = CARTESIAN_POINT ( 'NONE',  ( 0.006931111373678920488, 22.53293026234503316, 9.685942809247130469 ) ) ;
#12230 = CARTESIAN_POINT ( 'NONE',  ( 2.764680872515352661, -14.46287784598615644, -2.311161484776706576 ) ) ;
#12231 = EDGE_LOOP ( 'NONE', ( #363, #5115 ) ) ;
#12232 = AXIS2_PLACEMENT_3D ( 'NONE', #5783, #4640, #9320 ) ;
#12233 = VECTOR ( 'NONE', #4287, 1000.000000000000000 ) ;
#12234 = UNCERTAINTY_MEASURE_WITH_UNIT (LENGTH_MEASURE( 1.000000000000000082E-05 ), #1517, 'distance_accuracy_value', 'NONE');
#12235 = B_SPLINE_CURVE_WITH_KNOTS ( 'NONE', 3,
 ( #2729, #11932, #6028, #6971 ),
 .UNSPECIFIED., .F., .F.,
 ( 4, 4 ),
 ( 0.005123742438166228701, 0.005814376014856857504 ),
 .UNSPECIFIED. ) ;
#12236 = DIRECTION ( 'NONE',  ( -1.000000000000000000, 0.000000000000000000, 0.000000000000000000 ) ) ;
#12237 = ORIENTED_EDGE ( 'NONE', *, *, #10916, .T. ) ;
#12238 = DIRECTION ( 'NONE',  ( -1.000000000000000000, -0.000000000000000000, -0.000000000000000000 ) ) ;
#12239 = FACE_OUTER_BOUND ( 'NONE', #6337, .T. ) ;
#12240 = DIRECTION ( 'NONE',  ( -0.000000000000000000, -0.000000000000000000, -1.000000000000000000 ) ) ;
#12241 =( REPRESENTATION_RELATIONSHIP ('NONE','NONE', #12685, #7891 ) REPRESENTATION_RELATIONSHIP_WITH_TRANSFORMATION ( #13962 )SHAPE_REPRESENTATION_RELATIONSHIP( ) );
#12242 = AXIS2_PLACEMENT_3D ( 'NONE', #5213, #14269, #7507 ) ;
#12243 = AXIS2_PLACEMENT_3D ( 'NONE', #9109, #4121, #11328 ) ;
#12244 = AXIS2_PLACEMENT_3D ( 'NONE', #6036, #184, #4096 ) ;
#12245 = DIRECTION ( 'NONE',  ( 0.000000000000000000, 0.000000000000000000, -1.000000000000000000 ) ) ;
#12246 = EDGE_CURVE ( 'NONE', #12877, #1013, #15138, .T. ) ;
#12247 = FACE_BOUND ( 'NONE', #176, .T. ) ;
#12248 = EDGE_LOOP ( 'NONE', ( #964, #7704, #15136, #6676 ) ) ;
#12249 = DIRECTION ( 'NONE',  ( 0.000000000000000000, 0.000000000000000000, 1.000000000000000000 ) ) ;
#12250 = CARTESIAN_POINT ( 'NONE',  ( 2.764680872515352217, 2.311161484776756758, -14.46287784598614756 ) ) ;
#12251 = ORIENTED_EDGE ( 'NONE', *, *, #12834, .F. ) ;
#12252 = EDGE_LOOP ( 'NONE', ( #10377, #4437, #14426, #2058 ) ) ;
#12253 = SURFACE_STYLE_FILL_AREA ( #6183 ) ;
#12254 = FACE_OUTER_BOUND ( 'NONE', #14139, .T. ) ;
#12255 =( NAMED_UNIT ( * ) PLANE_ANGLE_UNIT ( ) SI_UNIT ( $, .RADIAN. ) );
#12256 = FACE_OUTER_BOUND ( 'NONE', #12623, .T. ) ;
#12257 = AXIS2_PLACEMENT_3D ( 'NONE', #13138, #222, #8154 ) ;
#12258 = CYLINDRICAL_SURFACE ( 'NONE', #4648, 13.19999999999999574 ) ;
#12259 = ORIENTED_EDGE ( 'NONE', *, *, #13760, .F. ) ;
#12260 = CARTESIAN_POINT ( 'NONE',  ( 2.789999999999999147, -2.311161484776655950, 14.46287784598616355 ) ) ;
#12261 = DIRECTION ( 'NONE',  ( 1.000000000000000000, 0.000000000000000000, 0.000000000000000000 ) ) ;
#12262 = CARTESIAN_POINT ( 'NONE',  ( 2.597943646031690257, -2.883512197588903092, -15.58455734132169468 ) ) ;
#12263 = CARTESIAN_POINT ( 'NONE',  ( 0.02436607992776498519, 9.836394144775706394, 22.71065055754456097 ) ) ;
#12264 = VERTEX_POINT ( 'NONE', #4523 ) ;
#12265 = AXIS2_PLACEMENT_3D ( 'NONE', #7063, #48, #3518 ) ;
#12266 = VERTEX_POINT ( 'NONE', #5609 ) ;
#12267 = ADVANCED_FACE ( 'NONE', ( #10207 ), #11357, .T. ) ;
#12268 = ORIENTED_EDGE ( 'NONE', *, *, #1399, .T. ) ;
#12269 = DIRECTION ( 'NONE',  ( -1.000000000000000000, -0.000000000000000000, -0.000000000000000000 ) ) ;
#12270 = DIRECTION ( 'NONE',  ( 0.000000000000000000, 0.000000000000000000, -1.000000000000000000 ) ) ;
#12271 = DIRECTION ( 'NONE',  ( 0.000000000000000000, 0.000000000000000000, 1.000000000000000000 ) ) ;
#12272 = CARTESIAN_POINT ( 'NONE',  ( 2.789999999999999147, 14.59528211760002137, -3.120158876139080828 ) ) ;
#12273 = PRODUCT_CONTEXT ( 'NONE', #6642, 'mechanical' ) ;
#12274 = CARTESIAN_POINT ( 'NONE',  ( 2.789999999999999147, -2.133490293296841589, -24.22479935914661198 ) ) ;
#12275 = CARTESIAN_POINT ( 'NONE',  ( 80.00000000000000000, 0.000000000000000000, 4.500000000000000888 ) ) ;
#12276 = CARTESIAN_POINT ( 'NONE',  ( 2.789999999999999147, -12.52067188844365830, 20.62201879784908698 ) ) ;
#12277 = PRODUCT_DEFINITION ( 'UNKNOWN', '', #14112, #1785 ) ;
#12278 = EDGE_CURVE ( 'NONE', #3477, #2567, #4375, .T. ) ;
#12279 = VERTEX_POINT ( 'NONE', #5461 ) ;
#12280 = DIRECTION ( 'NONE',  ( -0.000000000000000000, -0.000000000000000000, -1.000000000000000000 ) ) ;
#12281 = EDGE_CURVE ( 'NONE', #12104, #11073, #14643, .T. ) ;
#12282 = CARTESIAN_POINT ( 'NONE',  ( 3.751931928061364552, -0.6025004624012525456, 6.999999999999989342 ) ) ;
#12283 = DIRECTION ( 'NONE',  ( -1.000000000000000000, 0.000000000000000000, 0.000000000000000000 ) ) ;
#12284 = ORIENTED_EDGE ( 'NONE', *, *, #14445, .T. ) ;
#12285 = DIRECTION ( 'NONE',  ( -1.000000000000000000, -0.000000000000000000, -0.000000000000000000 ) ) ;
#12286 = LINE ( 'NONE', #1760, #14879 ) ;
#12287 = ORIENTED_EDGE ( 'NONE', *, *, #3826, .T. ) ;
#12288 = ORIENTED_EDGE ( 'NONE', *, *, #3772, .T. ) ;
#12289 = FILL_AREA_STYLE_COLOUR ( '', #2140 ) ;
#12290 = DIRECTION ( 'NONE',  ( 0.000000000000000000, 0.000000000000000000, 1.000000000000000000 ) ) ;
#12291 = CARTESIAN_POINT ( 'NONE',  ( 2.765633920072235075, -12.59161484032896361, -21.30679549418645280 ) ) ;
#12292 = DIRECTION ( 'NONE',  ( -1.000000000000000000, -0.000000000000000000, 0.000000000000000000 ) ) ;
#12293 = EDGE_CURVE ( 'NONE', #635, #2037, #6538, .T. ) ;
#12294 = DIRECTION ( 'NONE',  ( 1.000000000000000000, 0.000000000000000000, -2.710505431213761085E-17 ) ) ;
#12295 = EDGE_CURVE ( 'NONE', #4006, #4933, #3588, .T. ) ;
#12296 = CARTESIAN_POINT ( 'NONE',  ( 2.597943782557557757, 10.28947301956282345, 12.05486625177575455 ) ) ;
#12297 = EDGE_CURVE ( 'NONE', #7471, #13727, #8733, .T. ) ;
#12298 = ORIENTED_EDGE ( 'NONE', *, *, #4930, .T. ) ;
#12299 = CARTESIAN_POINT ( 'NONE',  ( 72.68384697807672978, 11.35494834827056110, 6.000000000000000000 ) ) ;
#12300 = DIRECTION ( 'NONE',  ( -0.000000000000000000, -0.000000000000000000, 1.000000000000000000 ) ) ;
#12301 = ADVANCED_FACE ( 'NONE', ( #3223 ), #13586, .T. ) ;
#12302 = ORIENTED_EDGE ( 'NONE', *, *, #5601, .F. ) ;
#12303 = ORIENTED_EDGE ( 'NONE', *, *, #6706, .T. ) ;
#12304 = ORIENTED_EDGE ( 'NONE', *, *, #4117, .T. ) ;
#12305 = CARTESIAN_POINT ( 'NONE',  ( 2.783025336474041378, -12.53640742967737332, -21.08118142846917209 ) ) ;
#12306 = DIRECTION ( 'NONE',  ( -1.000000000000000000, 0.000000000000000000, 0.000000000000000000 ) ) ;
#12307 = FACE_OUTER_BOUND ( 'NONE', #5419, .T. ) ;
#12308 = DIRECTION ( 'NONE',  ( -1.000000000000000000, -0.000000000000000000, -0.000000000000000000 ) ) ;
#12309 = ORIENTED_EDGE ( 'NONE', *, *, #14650, .T. ) ;
#12310 = CARTESIAN_POINT ( 'NONE',  ( -19.40394475573011590, -4.794738323547945491, 16.99999999999999645 ) ) ;
#12311 = CARTESIAN_POINT ( 'NONE',  ( -4.747884751462026820, -5.143694235355983579, -0.8000000000000000444 ) ) ;
#12312 = CARTESIAN_POINT ( 'NONE',  ( 2.789999999999999147, -1.948757464274075479, -13.87420763704363225 ) ) ;
#12313 = AXIS2_PLACEMENT_3D ( 'NONE', #4976, #3729, #7274 ) ;
#12314 = CARTESIAN_POINT ( 'NONE',  ( 2.718184749312773540, 2.576941577947758688, -25.22524549359947343 ) ) ;
#12315 = DIRECTION ( 'NONE',  ( -1.000000000000000000, -0.000000000000000000, 0.000000000000000000 ) ) ;
#12316 = VERTEX_POINT ( 'NONE', #10134 ) ;
#12317 = CARTESIAN_POINT ( 'NONE',  ( 0.01274102211100516108, 13.49735377262310720, -5.214906618939568084 ) ) ;
#12318 = CARTESIAN_POINT ( 'NONE',  ( 1.039999999999996705, -27.68468304288255410, -4.633866840649218055 ) ) ;
#12319 = ORIENTED_EDGE ( 'NONE', *, *, #12406, .T. ) ;
#12320 = EDGE_LOOP ( 'NONE', ( #8543, #14131, #7940, #2198, #14140, #6285, #640, #7139, #5409, #13588, #4227, #2345, #231, #7926, #4763, #5908, #4088, #7111, #13843, #6847, #5928, #8678, #7448, #14400, #10890, #11376, #2237, #6774, #10352, #6164, #2962, #8138, #2423, #570, #1562, #7992, #3699, #8800, #10500, #10027, #9783, #12953, #11689, #12472, #10857 ) ) ;
#12321 = FACE_BOUND ( 'NONE', #259, .T. ) ;
#12322 = CARTESIAN_POINT ( 'NONE',  ( 1.749999999999999778, -4.458161950358622505, 17.39253030560840330 ) ) ;
#12323 = AXIS2_PLACEMENT_3D ( 'NONE', #6911, #1067, #11658 ) ;
#12324 = CIRCLE ( 'NONE', #9623, 2.524999999999999467 ) ;
#12325 = FACE_OUTER_BOUND ( 'NONE', #13667, .T. ) ;
#12326 = CARTESIAN_POINT ( 'NONE',  ( 0.000000000000000000, 0.000000000000000000, 6.000000000000000000 ) ) ;
#12327 = DIRECTION ( 'NONE',  ( 1.000000000000000000, 0.000000000000000000, 0.000000000000000000 ) ) ;
#12328 = EDGE_CURVE ( 'NONE', #7552, #3308, #7768, .T. ) ;
#12329 = ORIENTED_EDGE ( 'NONE', *, *, #10787, .T. ) ;
#12330 = PLANE ( 'NONE',  #15114 ) ;
#12331 = DIRECTION ( 'NONE',  ( 1.000000000000000000, 0.000000000000000000, 0.000000000000000000 ) ) ;
#12332 = ORIENTED_EDGE ( 'NONE', *, *, #5705, .T. ) ;
#12333 = B_SPLINE_CURVE_WITH_KNOTS ( 'NONE', 3,
 ( #11405, #4353, #3128, #5440, #4503, #9184, #12635, #882 ),
 .UNSPECIFIED., .F., .F.,
 ( 4, 2, 2, 4 ),
 ( 4.663089416215518448E-07, 0.001898630173449453477, 0.002847712105703369741, 0.003796794037957286223 ),
 .UNSPECIFIED. ) ;
#12334 = LINE ( 'NONE', #10877, #14404 ) ;
#12335 = AXIS2_PLACEMENT_3D ( 'NONE', #9796, #3789, #11016 ) ;
#12336 = ORIENTED_EDGE ( 'NONE', *, *, #5155, .T. ) ;
#12337 = ORIENTED_EDGE ( 'NONE', *, *, #12667, .F. ) ;
#12338 = ORIENTED_EDGE ( 'NONE', *, *, #12835, .F. ) ;
#12339 = CARTESIAN_POINT ( 'NONE',  ( -14.40394475573011945, -10.79473832354794460, -5.000000000000000000 ) ) ;
#12340 = EDGE_CURVE ( 'NONE', #13265, #11577, #7907, .T. ) ;
#12341 = CARTESIAN_POINT ( 'NONE',  ( 2.257825491203655943, -24.44564404695836402, -11.58891744060133355 ) ) ;
#12342 = DIRECTION ( 'NONE',  ( 0.000000000000000000, 0.000000000000000000, -1.000000000000000000 ) ) ;
#12343 = APPLICATION_PROTOCOL_DEFINITION ( 'draft international standard', 'automotive_design', 1998, #10769 ) ;
#12344 = CARTESIAN_POINT ( 'NONE',  ( -5.209999999999999964, 0.000000000000000000, 0.000000000000000000 ) ) ;
#12345 = ADVANCED_FACE ( 'NONE', ( #759 ), #11426, .T. ) ;
#12346 = DIRECTION ( 'NONE',  ( 1.000000000000000000, 0.000000000000000000, 0.000000000000000000 ) ) ;
#12347 = CARTESIAN_POINT ( 'NONE',  ( -5.209999999999999964, 0.000000000000000000, 0.000000000000000000 ) ) ;
#12348 = VERTEX_POINT ( 'NONE', #14988 ) ;
#12349 = CARTESIAN_POINT ( 'NONE',  ( 2.021362756903528624, 4.022333916463829873, -17.00993931356757116 ) ) ;
#12350 = DIRECTION ( 'NONE',  ( 0.000000000000000000, 0.000000000000000000, 1.000000000000000000 ) ) ;
#12351 = EDGE_CURVE ( 'NONE', #6770, #1400, #6295, .T. ) ;
#12352 = FACE_OUTER_BOUND ( 'NONE', #9350, .T. ) ;
#12353 = ORIENTED_EDGE ( 'NONE', *, *, #5999, .F. ) ;
#12354 = DIRECTION ( 'NONE',  ( -1.000000000000000000, -0.000000000000000000, 0.000000000000000000 ) ) ;
#12355 = DIRECTION ( 'NONE',  ( 0.000000000000000000, 0.000000000000000000, 1.000000000000000000 ) ) ;
#12356 = ORIENTED_EDGE ( 'NONE', *, *, #8570, .T. ) ;
#12357 = ORIENTED_EDGE ( 'NONE', *, *, #4984, .F. ) ;
#12358 = DIRECTION ( 'NONE',  ( -0.000000000000000000, -0.000000000000000000, -1.000000000000000000 ) ) ;
#12359 = CARTESIAN_POINT ( 'NONE',  ( 0.1587402281127123227, 22.38003579136345067, 12.81821841996081801 ) ) ;
#12360 = EDGE_CURVE ( 'NONE', #949, #12913, #6824, .T. ) ;
#12361 = EDGE_CURVE ( 'NONE', #6679, #1826, #6787, .T. ) ;
#12362 = CARTESIAN_POINT ( 'NONE',  ( 1.749999999999998002, 19.67366047555530528, 20.02152543075352753 ) ) ;
#12363 = DIRECTION ( 'NONE',  ( 0.4036950204470267645, -0.9148936170212768060, 0.000000000000000000 ) ) ;
#12364 = CARTESIAN_POINT ( 'NONE',  ( 2.789999999999999147, 0.000000000000000000, 0.000000000000000000 ) ) ;
#12365 = CARTESIAN_POINT ( 'NONE',  ( 1.039999999999994929, -25.12109765559662833, 12.52377138324214023 ) ) ;
#12366 = LINE ( 'NONE', #7847, #3260 ) ;
#12367 = ORIENTED_EDGE ( 'NONE', *, *, #14823, .F. ) ;
#12368 = DIRECTION ( 'NONE',  ( 1.000000000000000000, 0.000000000000000000, 0.000000000000000000 ) ) ;
#12369 = VECTOR ( 'NONE', #9557, 1000.000000000000000 ) ;
#12370 = AXIS2_PLACEMENT_3D ( 'NONE', #13455, #12457, #1704 ) ;
#12371 = DIRECTION ( 'NONE',  ( -1.000000000000000000, 0.000000000000000000, 0.000000000000000000 ) ) ;
#12372 = VECTOR ( 'NONE', #8205, 1000.000000000000000 ) ;
#12373 = ORIENTED_EDGE ( 'NONE', *, *, #4133, .F. ) ;
#12374 = EDGE_CURVE ( 'NONE', #13280, #12872, #14149, .T. ) ;
#12375 = VERTEX_POINT ( 'NONE', #1834 ) ;
#12376 = ORIENTED_EDGE ( 'NONE', *, *, #11239, .F. ) ;
#12377 = ORIENTED_EDGE ( 'NONE', *, *, #1603, .T. ) ;
#12378 = CARTESIAN_POINT ( 'NONE',  ( 2.764680872513682885, -14.46287784598619020, 2.311161484776505404 ) ) ;
#12379 = CIRCLE ( 'NONE', #1829, 4.599999999999999645 ) ;
#12380 = ADVANCED_FACE ( 'NONE', ( #6524 ), #11206, .F. ) ;
#12381 = DIRECTION ( 'NONE',  ( 0.000000000000000000, 0.000000000000000000, -1.000000000000000000 ) ) ;
#12382 = EDGE_CURVE ( 'NONE', #9979, #7272, #1058, .T. ) ;
#12383 = AXIS2_PLACEMENT_3D ( 'NONE', #14834, #2149, #11296 ) ;
#12384 = CIRCLE ( 'NONE', #13102, 3.000000000000002665 ) ;
#12385 = PRODUCT_DEFINITION_CONTEXT ( 'detailed design', #3485, 'design' ) ;
#12386 = CYLINDRICAL_SURFACE ( 'NONE', #13474, 28.06981291497571362 ) ;
#12387 = CARTESIAN_POINT ( 'NONE',  ( 0.02436607992775934733, -21.30679549418640306, 12.59161484032904887 ) ) ;
#12388 = VERTEX_POINT ( 'NONE', #3368 ) ;
#12389 = CARTESIAN_POINT ( 'NONE',  ( 0.02531912748464631296, -13.68080036884344963, -5.229914364928496262 ) ) ;
#12390 = CARTESIAN_POINT ( 'NONE',  ( 0.02436607992776108206, -24.15498966839966855, 5.391175441198523544 ) ) ;
#12391 = AXIS2_PLACEMENT_3D ( 'NONE', #11640, #10726, #4901 ) ;
#12392 = AXIS2_PLACEMENT_3D ( 'NONE', #10243, #11538, #14859 ) ;
#12393 = CARTESIAN_POINT ( 'NONE',  ( -1.150000000000000577, 0.000000000000000000, 0.000000000000000000 ) ) ;
#12394 = AXIS2_PLACEMENT_3D ( 'NONE', #8234, #2482, #230 ) ;
#12395 = DIRECTION ( 'NONE',  ( 0.000000000000000000, 0.000000000000000000, 1.000000000000000000 ) ) ;
#12396 = B_SPLINE_CURVE_WITH_KNOTS ( 'NONE', 3,
 ( #3301, #9223, #14920, #13759, #7764, #7688, #3234, #10368 ),
 .UNSPECIFIED., .F., .F.,
 ( 4, 2, 2, 4 ),
 ( 2.032124546189621919E-07, 0.001631739532304474910, 0.002447507692229407717, 0.003263275852154340524 ),
 .UNSPECIFIED. ) ;
#12397 = EDGE_LOOP ( 'NONE', ( #825, #6727, #7192, #6353 ) ) ;
#12398 = CARTESIAN_POINT ( 'NONE',  ( 0.02531912748605881155, 13.68080036884355621, -5.229914364928207604 ) ) ;
#12399 = CARTESIAN_POINT ( 'NONE',  ( -7.928732286808572430E-16, 18.34424029220111052, 15.96500990068130577 ) ) ;
#12400 = VERTEX_POINT ( 'NONE', #404 ) ;
#12401 = ORIENTED_EDGE ( 'NONE', *, *, #4883, .T. ) ;
#12402 = CIRCLE ( 'NONE', #11898, 9.999999999999994671 ) ;
#12403 = AXIS2_PLACEMENT_3D ( 'NONE', #6011, #8544, #9698 ) ;
#12404 = CIRCLE ( 'NONE', #7748, 2.524999999999999023 ) ;
#12405 = CYLINDRICAL_SURFACE ( 'NONE', #13869, 2.524999999999995914 ) ;
#12406 = EDGE_CURVE ( 'NONE', #7326, #5643, #390, .T. ) ;
#12407 = EDGE_LOOP ( 'NONE', ( #9114, #10496, #21, #11755 ) ) ;
#12408 = CARTESIAN_POINT ( 'NONE',  ( 2.789999999999999147, -11.36963888406694068, 9.232963481057725019 ) ) ;
#12409 = ORIENTED_EDGE ( 'NONE', *, *, #3772, .F. ) ;
#12410 = LINE ( 'NONE', #3264, #14381 ) ;
#12411 = CARTESIAN_POINT ( 'NONE',  ( 13.45237873341251067, -22.10506396614762537, 2.000000000000000000 ) ) ;
#12412 = ORIENTED_EDGE ( 'NONE', *, *, #420, .F. ) ;
#12413 = VECTOR ( 'NONE', #6298, 1000.000000000000000 ) ;
#12414 = CARTESIAN_POINT ( 'NONE',  ( 0.5279272933715190019, 18.56460150496967287, -19.66369668717012331 ) ) ;
#12415 = VERTEX_POINT ( 'NONE', #3441 ) ;
#12416 = VERTEX_POINT ( 'NONE', #6255 ) ;
#12417 = ORIENTED_EDGE ( 'NONE', *, *, #321, .T. ) ;
#12418 = LINE ( 'NONE', #8880, #9262 ) ;
#12419 = CARTESIAN_POINT ( 'NONE',  ( 1.039999999999996705, -27.68468304288255410, -4.633866840649218055 ) ) ;
#12420 = EDGE_CURVE ( 'NONE', #11060, #7248, #8057, .T. ) ;
#12421 = CIRCLE ( 'NONE', #14652, 5.999999999999999112 ) ;
#12422 = FACE_OUTER_BOUND ( 'NONE', #1367, .T. ) ;
#12423 = DIRECTION ( 'NONE',  ( -1.000000000000000000, 0.000000000000000000, 0.000000000000000000 ) ) ;
#12424 = DIRECTION ( 'NONE',  ( 0.000000000000000000, 0.000000000000000000, 1.000000000000000000 ) ) ;
#12425 = DIRECTION ( 'NONE',  ( 0.4571871344001384174, 0.8893705212896307888, 0.000000000000000000 ) ) ;
#12426 = B_SPLINE_CURVE_WITH_KNOTS ( 'NONE', 3,
 ( #14529, #10901, #515, #3837, #3992, #14458, #8664, #14600 ),
 .UNSPECIFIED., .F., .F.,
 ( 4, 2, 2, 4 ),
 ( 4.663089412835749521E-07, 0.001898630173449111953, 0.002847712105703030603, 0.003796794037956948819 ),
 .UNSPECIFIED. ) ;
#12427 = PRESENTATION_LAYER_ASSIGNMENT (  '', '', ( #11447 ) ) ;
#12428 = DIRECTION ( 'NONE',  ( -1.000000000000000000, -0.000000000000000000, -0.000000000000000000 ) ) ;
#12429 = CARTESIAN_POINT ( 'NONE',  ( -20.63749999999999574, 0.000000000000000000, -5.575000000000000178 ) ) ;
#12430 = ORIENTED_EDGE ( 'NONE', *, *, #2054, .F. ) ;
#12431 = CARTESIAN_POINT ( 'NONE',  ( 1.249999999999997558, 0.000000000000000000, -4.424999999999999822 ) ) ;
#12432 = LINE ( 'NONE', #896, #526 ) ;
#12433 = CARTESIAN_POINT ( 'NONE',  ( 0.02436607992776325046, -24.15498966839958683, -5.391175441198872598 ) ) ;
#12434 = EDGE_CURVE ( 'NONE', #8724, #10827, #12235, .T. ) ;
#12435 = AXIS2_PLACEMENT_3D ( 'NONE', #9417, #2440, #105 ) ;
#12436 = AXIS2_PLACEMENT_3D ( 'NONE', #8156, #1309, #14235 ) ;
#12437 = ORIENTED_EDGE ( 'NONE', *, *, #2396, .F. ) ;
#12438 = EDGE_CURVE ( 'NONE', #3623, #9529, #4084, .T. ) ;
#12439 = CARTESIAN_POINT ( 'NONE',  ( -10.00000000000000000, 0.000000000000000000, 0.000000000000000000 ) ) ;
#12440 = DIRECTION ( 'NONE',  ( -0.000000000000000000, -0.000000000000000000, 1.000000000000000000 ) ) ;
#12441 = ORIENTED_EDGE ( 'NONE', *, *, #5870, .T. ) ;
#12442 = CIRCLE ( 'NONE', #11209, 14.01039946648073986 ) ;
#12443 = CIRCLE ( 'NONE', #12676, 2.524999999999995914 ) ;
#12444 = ORIENTED_EDGE ( 'NONE', *, *, #1857, .F. ) ;
#12445 = DIRECTION ( 'NONE',  ( -0.000000000000000000, -0.000000000000000000, 1.000000000000000000 ) ) ;
#12446 = CYLINDRICAL_SURFACE ( 'NONE', #12211, 28.06981291497571362 ) ;
#12447 = CARTESIAN_POINT ( 'NONE',  ( -17.28189153115278032, -8.313322929496736791, 0.7999999999999961586 ) ) ;
#12448 = DIRECTION ( 'NONE',  ( 1.000000000000000000, 1.445602896647338917E-16, 0.000000000000000000 ) ) ;
#12449 = FACE_OUTER_BOUND ( 'NONE', #3131, .T. ) ;
#12450 = AXIS2_PLACEMENT_3D ( 'NONE', #9205, #2215, #8411 ) ;
#12451 = CARTESIAN_POINT ( 'NONE',  ( 0.02436607992776411782, 22.71065055754465689, -9.836394144775473691 ) ) ;
#12452 = CARTESIAN_POINT ( 'NONE',  ( 1.394999999999999574, -4.835383649608592016, 17.29145405592687368 ) ) ;
#12453 = VERTEX_POINT ( 'NONE', #9209 ) ;
#12454 = DIRECTION ( 'NONE',  ( -0.4055247608874392173, 0.9140840597599244610, -7.389059384413458221E-17 ) ) ;
#12455 = COLOUR_RGB ( '',0.8941176470588234615, 0.8941176470588234615, 0.8941176470588234615 ) ;
#12456 = CIRCLE ( 'NONE', #14424, 2.524999999999994582 ) ;
#12457 = DIRECTION ( 'NONE',  ( -0.000000000000000000, -0.000000000000000000, -1.000000000000000000 ) ) ;
#12458 = VECTOR ( 'NONE', #9604, 1000.000000000000000 ) ;
#12459 = ORIENTED_EDGE ( 'NONE', *, *, #14066, .F. ) ;
#12460 = ORIENTED_EDGE ( 'NONE', *, *, #6765, .T. ) ;
#12461 = ORIENTED_EDGE ( 'NONE', *, *, #13802, .F. ) ;
#12462 = ORIENTED_EDGE ( 'NONE', *, *, #10519, .F. ) ;
#12463 = CARTESIAN_POINT ( 'NONE',  ( 4.271534284832219323E-17, 3.369532131271296443E-15, 6.999999999999989342 ) ) ;
#12464 = DIRECTION ( 'NONE',  ( 1.000000000000000000, 0.000000000000000000, -0.000000000000000000 ) ) ;
#12465 = EDGE_CURVE ( 'NONE', #677, #11238, #12659, .T. ) ;
#12466 = MECHANICAL_DESIGN_GEOMETRIC_PRESENTATION_REPRESENTATION (  '', ( #10019 ), #10754 ) ;
#12467 = VECTOR ( 'NONE', #3351, 1000.000000000000000 ) ;
#12468 = AXIS2_PLACEMENT_3D ( 'NONE', #7516, #5150, #3905 ) ;
#12469 = VECTOR ( 'NONE', #4101, 1000.000000000000000 ) ;
#12470 = DIRECTION ( 'NONE',  ( -1.000000000000000000, 0.000000000000000000, 0.000000000000000000 ) ) ;
#12471 = DIRECTION ( 'NONE',  ( 1.000000000000000000, 0.000000000000000000, 0.000000000000000000 ) ) ;
#12472 = ORIENTED_EDGE ( 'NONE', *, *, #11067, .F. ) ;
#12473 = CARTESIAN_POINT ( 'NONE',  ( 0.02531912748464804769, 9.232963481057765875, 11.36963888406690870 ) ) ;
#12474 = LINE ( 'NONE', #9859, #12469 ) ;
#12475 = EDGE_CURVE ( 'NONE', #1743, #12123, #14641, .T. ) ;
#12476 = ADVANCED_FACE ( 'NONE', ( #2217 ), #10435, .T. ) ;
#12477 = AXIS2_PLACEMENT_3D ( 'NONE', #600, #12128, #1620 ) ;
#12478 = DIRECTION ( 'NONE',  ( -1.000000000000000000, 0.000000000000000000, 0.000000000000000000 ) ) ;
#12479 = VECTOR ( 'NONE', #14258, 1000.000000000000000 ) ;
#12480 = AXIS2_PLACEMENT_3D ( 'NONE', #800, #3038, #652 ) ;
#12481 = EDGE_LOOP ( 'NONE', ( #13258, #13002, #870, #5685 ) ) ;
#12482 = CARTESIAN_POINT ( 'NONE',  ( 1.666666666666673624, 0.000000000000000000, 3.000000000000002665 ) ) ;
#12483 = DIRECTION ( 'NONE',  ( 0.000000000000000000, 0.000000000000000000, 1.000000000000000000 ) ) ;
#12484 = ORIENTED_EDGE ( 'NONE', *, *, #7425, .F. ) ;
#12485 = EDGE_LOOP ( 'NONE', ( #12373, #1328, #10324, #14223 ) ) ;
#12486 = LINE ( 'NONE', #5361, #3639 ) ;
#12487 =( NAMED_UNIT ( * ) PLANE_ANGLE_UNIT ( ) SI_UNIT ( $, .RADIAN. ) );
#12488 = CARTESIAN_POINT ( 'NONE',  ( 0.000000000000000000, 5.535312321043032391, -23.48180575137725867 ) ) ;
#12489 = EDGE_CURVE ( 'NONE', #1588, #7234, #8558, .T. ) ;
#12490 = EDGE_CURVE ( 'NONE', #11633, #11133, #9290, .T. ) ;
#12491 = ORIENTED_EDGE ( 'NONE', *, *, #3845, .F. ) ;
#12492 = CARTESIAN_POINT ( 'NONE',  ( 0.000000000000000000, 1.991882183130315953, 24.04302995059967074 ) ) ;
#12493 = AXIS2_PLACEMENT_3D ( 'NONE', #49, #11662, #12815 ) ;
#12494 = AXIS2_PLACEMENT_3D ( 'NONE', #410, #1575, #3803 ) ;
#12495 = AXIS2_PLACEMENT_3D ( 'NONE', #8045, #1203, #10577 ) ;
#12497 = VERTEX_POINT ( 'NONE', #3793 ) ;
#12496 = EDGE_CURVE ( 'NONE', #6903, #5629, #1374, .T. ) ;
#12498 = DIRECTION ( 'NONE',  ( 0.000000000000000000, 0.000000000000000000, 1.000000000000000000 ) ) ;
#12499 = VERTEX_POINT ( 'NONE', #13076 ) ;
#12500 = SURFACE_STYLE_FILL_AREA ( #7814 ) ;
#12501 = CARTESIAN_POINT ( 'NONE',  ( -14.40394475573011945, -10.79473832354794460, -3.000000000000000000 ) ) ;
#12502 = ORIENTED_EDGE ( 'NONE', *, *, #630, .T. ) ;
#12503 = EDGE_CURVE ( 'NONE', #13379, #3242, #11652, .T. ) ;
#12504 = ORIENTED_EDGE ( 'NONE', *, *, #13238, .T. ) ;
#12505 =( NAMED_UNIT ( * ) SI_UNIT ( $, .STERADIAN. ) SOLID_ANGLE_UNIT ( ) );
#12506 = CIRCLE ( 'NONE', #2701, 4.000000000000003553 ) ;
#12507 = DIRECTION ( 'NONE',  ( -5.480158469902919838E-17, -1.051478716308701618E-16, -1.000000000000000000 ) ) ;
#12508 = CARTESIAN_POINT ( 'NONE',  ( 0.02436607992776455150, -22.71065055754459650, 9.836394144775621129 ) ) ;
#12509 = LINE ( 'NONE', #813, #1602 ) ;
#12510 = CARTESIAN_POINT ( 'NONE',  ( 0.02436607992776411782, -16.37294372382844543, -18.55949924794910544 ) ) ;
#12511 = DIRECTION ( 'NONE',  ( 0.000000000000000000, 0.000000000000000000, 1.000000000000000000 ) ) ;
#12512 = VERTEX_POINT ( 'NONE', #7260 ) ;
#12513 = CARTESIAN_POINT ( 'NONE',  ( 2.582362678678089551, 2.899259574942964157, -15.57879356040259822 ) ) ;
#12514 = CARTESIAN_POINT ( 'NONE',  ( -16.02604379927987566, -7.138402084508245871, -3.800000000000000266 ) ) ;
#12515 = CIRCLE ( 'NONE', #3187, 3.799999999999999378 ) ;
#12516 = CARTESIAN_POINT ( 'NONE',  ( 79.18363542992867110, -10.13606076167855008, 7.000000000000000000 ) ) ;
#12517 = ORIENTED_EDGE ( 'NONE', *, *, #3715, .F. ) ;
#12518 = CARTESIAN_POINT ( 'NONE',  ( 2.789999999999999147, -7.909232158574647009, -21.81711360614308148 ) ) ;
#12519 = CARTESIAN_POINT ( 'NONE',  ( 80.82762530298222714, -9.999999999999994671, 4.000000000000003553 ) ) ;
#12520 = EDGE_LOOP ( 'NONE', ( #284, #536 ) ) ;
#12521 = VERTEX_POINT ( 'NONE', #6111 ) ;
#12522 = CARTESIAN_POINT ( 'NONE',  ( 0.000000000000000000, 0.000000000000000000, 0.000000000000000000 ) ) ;
#12523 = FACE_OUTER_BOUND ( 'NONE', #1713, .T. ) ;
#12524 = EDGE_LOOP ( 'NONE', ( #4944, #194, #983, #8804 ) ) ;
#12525 = FACE_OUTER_BOUND ( 'NONE', #7084, .T. ) ;
#12526 = CARTESIAN_POINT ( 'NONE',  ( -18.40394475573011945, -10.79473832354794460, -5.000000000000000000 ) ) ;
#12527 = CARTESIAN_POINT ( 'NONE',  ( -17.10144940350364706, -13.74829019802725050, 0.7999999999999960476 ) ) ;
#12528 = DIRECTION ( 'NONE',  ( 0.000000000000000000, 0.4999999999999891198, 0.8660254037844450359 ) ) ;
#12529 = CARTESIAN_POINT ( 'NONE',  ( 2.789999999999999147, 5.456805104201435164, -23.69843731927162978 ) ) ;
#12530 = ORIENTED_EDGE ( 'NONE', *, *, #12208, .T. ) ;
#12531 = CARTESIAN_POINT ( 'NONE',  ( -1.150000000000001688, 7.347880794884120722E-16, 6.000000000000001776 ) ) ;
#12532 = DIRECTION ( 'NONE',  ( -0.000000000000000000, -0.000000000000000000, -1.000000000000000000 ) ) ;
#12533 = EDGE_LOOP ( 'NONE', ( #402, #7346 ) ) ;
#12534 = ORIENTED_EDGE ( 'NONE', *, *, #9872, .F. ) ;
#12535 = ORIENTED_EDGE ( 'NONE', *, *, #11618, .F. ) ;
#12536 = ORIENTED_EDGE ( 'NONE', *, *, #9421, .F. ) ;
#12537 = DIRECTION ( 'NONE',  ( 1.000000000000000000, 0.000000000000000000, 0.000000000000000000 ) ) ;
#12538 = CARTESIAN_POINT ( 'NONE',  ( 3.321103546710217902, -13.95673088054953759, 4.000000000000000000 ) ) ;
#12539 = CARTESIAN_POINT ( 'NONE',  ( 2.765633920072239071, -12.59161484032927092, 21.30679549418627161 ) ) ;
#12540 = EDGE_CURVE ( 'NONE', #6652, #7725, #6550, .T. ) ;
#12541 = ORIENTED_EDGE ( 'NONE', *, *, #5772, .T. ) ;
#12542 = B_SPLINE_CURVE_WITH_KNOTS ( 'NONE', 3,
 ( #5687, #9139, #15139, #13897, #14912, #14993 ),
 .UNSPECIFIED., .F., .F.,
 ( 4, 2, 4 ),
 ( 2.132675795048140432E-07, 0.001878604073277005205, 0.003756994878974505639 ),
 .UNSPECIFIED. ) ;
#12543 = PLANE ( 'NONE',  #10176 ) ;
#12544 = DIRECTION ( 'NONE',  ( -1.445602896647338917E-16, 1.000000000000000000, -0.000000000000000000 ) ) ;
#12545 = CARTESIAN_POINT ( 'NONE',  ( 2.789999999999999147, -12.98979500319690317, -5.249430348645892863 ) ) ;
#12546 = EDGE_CURVE ( 'NONE', #9595, #8589, #13409, .T. ) ;
#12547 = DIRECTION ( 'NONE',  ( -0.000000000000000000, -0.000000000000000000, 1.000000000000000000 ) ) ;
#12548 = VERTEX_POINT ( 'NONE', #5042 ) ;
#12549 = CARTESIAN_POINT ( 'NONE',  ( 98.48580539929344013, 0.9022481406819604643, 6.000000000000000000 ) ) ;
#12550 = CARTESIAN_POINT ( 'NONE',  ( 2.765633920072235963, -24.63872515616080960, -2.336989772644527008 ) ) ;
#12551 = ORIENTED_EDGE ( 'NONE', *, *, #6906, .T. ) ;
#12552 = ORIENTED_EDGE ( 'NONE', *, *, #15030, .F. ) ;
#12553 = EDGE_CURVE ( 'NONE', #7105, #12050, #9715, .T. ) ;
#12554 = EDGE_CURVE ( 'NONE', #1582, #3392, #9482, .T. ) ;
#12555 =( LENGTH_UNIT ( ) NAMED_UNIT ( * ) SI_UNIT ( .MILLI., .METRE. ) );
#12556 = CARTESIAN_POINT ( 'NONE',  ( 2.765633920072239516, -2.336989772644097574, -24.63872515616085224 ) ) ;
#12557 = ORIENTED_EDGE ( 'NONE', *, *, #5267, .F. ) ;
#12558 = CARTESIAN_POINT ( 'NONE',  ( 86.17559721729969624, 12.01344854909570259, 6.000000000000000000 ) ) ;
#12559 = ORIENTED_EDGE ( 'NONE', *, *, #14781, .T. ) ;
#12560 = DIRECTION ( 'NONE',  ( 0.000000000000000000, 0.000000000000000000, 1.000000000000000000 ) ) ;
#12561 = CARTESIAN_POINT ( 'NONE',  ( -14.40394475573011945, -10.79473832354794460, -5.000000000000000000 ) ) ;
#12562 = ORIENTED_EDGE ( 'NONE', *, *, #3451, .F. ) ;
#12563 = B_SPLINE_CURVE_WITH_KNOTS ( 'NONE', 3,
 ( #12721, #9278, #12790, #2277 ),
 .UNSPECIFIED., .F., .F.,
 ( 4, 4 ),
 ( 2.159563976993877881E-07, 0.0006916893629248557470 ),
 .UNSPECIFIED. ) ;
#12564 = DIRECTION ( 'NONE',  ( 0.000000000000000000, 0.000000000000000000, 1.000000000000000000 ) ) ;
#12565 = CARTESIAN_POINT ( 'NONE',  ( 2.765633920072238627, 12.59161484032942901, -21.30679549418617924 ) ) ;
#12566 = ORIENTED_EDGE ( 'NONE', *, *, #2983, .F. ) ;
#12567 = EDGE_CURVE ( 'NONE', #15052, #5963, #7282, .T. ) ;
#12568 = ORIENTED_EDGE ( 'NONE', *, *, #11578, .F. ) ;
#12569 = CARTESIAN_POINT ( 'NONE',  ( 85.79342132543153809, 17.83186255874426962, 2.999999999999999112 ) ) ;
#12570 = DIRECTION ( 'NONE',  ( -0.5416238976136773520, 0.8406209333187990573, 0.000000000000000000 ) ) ;
#12571 = EDGE_CURVE ( 'NONE', #5551, #8235, #5286, .T. ) ;
#12572 = DIRECTION ( 'NONE',  ( 1.000000000000000000, 0.000000000000000000, 0.000000000000000000 ) ) ;
#12573 = CARTESIAN_POINT ( 'NONE',  ( 2.789999999999999147, 5.535312321042718864, 23.48180575137732262 ) ) ;
#12574 = ITEM_DEFINED_TRANSFORMATION ( 'NONE', 'NONE', #2544,  #1376 ) ;
#12575 = LINE ( 'NONE', #2049, #3655 ) ;
#12576 = CARTESIAN_POINT ( 'NONE',  ( 2.790000000000061320, 13.12794558796753819, -5.226347720069123071 ) ) ;
#12577 = EDGE_CURVE ( 'NONE', #7883, #3989, #13551, .T. ) ;
#12578 = ORIENTED_EDGE ( 'NONE', *, *, #7788, .F. ) ;
#12579 = DIRECTION ( 'NONE',  ( 0.000000000000000000, 0.000000000000000000, 1.000000000000000000 ) ) ;
#12580 = DIRECTION ( 'NONE',  ( -1.000000000000000000, -0.000000000000000000, -0.000000000000000000 ) ) ;
#12581 = DIRECTION ( 'NONE',  ( -1.000000000000000000, -0.000000000000000000, 0.000000000000000000 ) ) ;
#12582 = VERTEX_POINT ( 'NONE', #7642 ) ;
#12583 = CARTESIAN_POINT ( 'NONE',  ( 2.789999999999999147, -14.46287784598615644, -2.311161484776706576 ) ) ;
#12584 = CARTESIAN_POINT ( 'NONE',  ( 2.765633920072238627, 5.391175441198956086, -24.15498966839956907 ) ) ;
#12585 = ORIENTED_EDGE ( 'NONE', *, *, #5405, .F. ) ;
#12586 = ORIENTED_EDGE ( 'NONE', *, *, #1967, .F. ) ;
#12587 = DIRECTION ( 'NONE',  ( 0.000000000000000000, 0.000000000000000000, 1.000000000000000000 ) ) ;
#12588 = CARTESIAN_POINT ( 'NONE',  ( 2.782672486186224425, -5.204526028255594738, -13.44898112152243819 ) ) ;
#12589 = ORIENTED_EDGE ( 'NONE', *, *, #2587, .F. ) ;
#12590 = CARTESIAN_POINT ( 'NONE',  ( 1.039999999999997593, 0.000000000000000000, 0.000000000000000000 ) ) ;
#12591 = CARTESIAN_POINT ( 'NONE',  ( 9.603018496175287840E-16, -5.456805104200934231, -23.69843731927176123 ) ) ;
#12592 = FILL_AREA_STYLE ('',( #7916 ) ) ;
#12593 = DIRECTION ( 'NONE',  ( 1.000000000000000000, 0.000000000000000000, 0.000000000000000000 ) ) ;
#12594 = CARTESIAN_POINT ( 'NONE',  ( -6.099252894168396215E-14, -8.842064619038449536, -11.12234047011199500 ) ) ;
#12595 = EDGE_CURVE ( 'NONE', #672, #5459, #11926, .T. ) ;
#12596 = ORIENTED_EDGE ( 'NONE', *, *, #13476, .F. ) ;
#12597 = DIRECTION ( 'NONE',  ( -1.000000000000000000, -0.000000000000000000, -0.000000000000000000 ) ) ;
#12598 = CARTESIAN_POINT ( 'NONE',  ( 2.783069004973548033, 23.92277630352795370, 5.408431875071527450 ) ) ;
#12599 = ORIENTED_EDGE ( 'NONE', *, *, #7651, .T. ) ;
#12600 = DIRECTION ( 'NONE',  ( 0.000000000000000000, 0.000000000000000000, 1.000000000000000000 ) ) ;
#12601 = ORIENTED_EDGE ( 'NONE', *, *, #9356, .T. ) ;
#12602 = VERTEX_POINT ( 'NONE', #4188 ) ;
#12603 = VERTEX_POINT ( 'NONE', #13395 ) ;
#12604 = CARTESIAN_POINT ( 'NONE',  ( -9.970929402304026638E-15, -5.211150952915271084, -13.21889893246980918 ) ) ;
#12605 = PRODUCT_DEFINITION_FORMATION_WITH_SPECIFIED_SOURCE ( 'ANY', '', #6388, .NOT_KNOWN. ) ;
#12606 = CARTESIAN_POINT ( 'NONE',  ( 2.246812850058910183, -5.154374911958798933, -16.16568790143447032 ) ) ;
#12607 = ADVANCED_FACE ( 'NONE', ( #8858 ), #1647, .T. ) ;
#12608 = CARTESIAN_POINT ( 'NONE',  ( 0.000000000000000000, -8.624777288397881492, 11.04103753892268891 ) ) ;
#12609 = ORIENTED_EDGE ( 'NONE', *, *, #1840, .T. ) ;
#12610 = AXIS2_PLACEMENT_3D ( 'NONE', #8137, #2525, #205 ) ;
#12611 = CARTESIAN_POINT ( 'NONE',  ( 0.000000000000000000, 0.000000000000000000, 0.000000000000000000 ) ) ;
#12612 = LINE ( 'NONE', #5566, #1675 ) ;
#12613 = DIRECTION ( 'NONE',  ( 0.000000000000000000, 0.000000000000000000, 1.000000000000000000 ) ) ;
#12614 = AXIS2_PLACEMENT_3D ( 'NONE', #7462, #13527, #766 ) ;
#12615 = EDGE_CURVE ( 'NONE', #14375, #3154, #8014, .T. ) ;
#12616 = AXIS2_PLACEMENT_3D ( 'NONE', #12219, #2619, #7315 ) ;
#12617 = AXIS2_PLACEMENT_3D ( 'NONE', #9079, #2007, #5550 ) ;
#12618 = VERTEX_POINT ( 'NONE', #5271 ) ;
#12619 = DIRECTION ( 'NONE',  ( 1.000000000000000000, 0.000000000000000000, 0.000000000000000000 ) ) ;
#12620 = ADVANCED_FACE ( 'NONE', ( #482 ), #1876, .T. ) ;
#12621 = CARTESIAN_POINT ( 'NONE',  ( 70.16198417812034904, 9.730076655429538590, 4.000000000000000000 ) ) ;
#12622 = ORIENTED_EDGE ( 'NONE', *, *, #10568, .T. ) ;
#12623 = EDGE_LOOP ( 'NONE', ( #13064, #4497, #13298, #8217, #3510, #4456, #6181 ) ) ;
#12624 = DIRECTION ( 'NONE',  ( -1.000000000000000000, -0.000000000000000000, -0.000000000000000000 ) ) ;
#12625 = AXIS2_PLACEMENT_3D ( 'NONE', #183, #8184, #1123 ) ;
#12626 = CIRCLE ( 'NONE', #604, 28.06981291497571362 ) ;
#12627 = VERTEX_POINT ( 'NONE', #3026 ) ;
#12628 = COLOUR_RGB ( '',0.8941176470588234615, 0.8941176470588234615, 0.8941176470588234615 ) ;
#12629 = DIRECTION ( 'NONE',  ( -1.000000000000000000, 0.000000000000000000, 0.000000000000000000 ) ) ;
#12630 = CYLINDRICAL_SURFACE ( 'NONE', #8465, 13.19999999999999929 ) ;
#12631 = CYLINDRICAL_SURFACE ( 'NONE', #14796, 3.799999999999999378 ) ;
#12632 = ORIENTED_EDGE ( 'NONE', *, *, #3417, .F. ) ;
#12633 = CARTESIAN_POINT ( 'NONE',  ( 2.789999999999999147, -7.909232158574988958, 24.34211360614297348 ) ) ;
#12634 = EDGE_CURVE ( 'NONE', #5235, #13626, #2625, .T. ) ;
#12635 = CARTESIAN_POINT ( 'NONE',  ( 0.04999671152047786143, 2.439987328296971736, 14.75565684666128163 ) ) ;
#12636 = PRODUCT_DEFINITION_FORMATION_WITH_SPECIFIED_SOURCE ( 'ANY', '', #14394, .NOT_KNOWN. ) ;
#12637 = ORIENTED_EDGE ( 'NONE', *, *, #4222, .F. ) ;
#12638 = AXIS2_PLACEMENT_3D ( 'NONE', #12697, #12838, #10554 ) ;
#12639 = ORIENTED_EDGE ( 'NONE', *, *, #6906, .F. ) ;
#12640 =( LENGTH_UNIT ( ) NAMED_UNIT ( * ) SI_UNIT ( .MILLI., .METRE. ) );
#12641 = FACE_OUTER_BOUND ( 'NONE', #9564, .T. ) ;
#12642 = EDGE_CURVE ( 'NONE', #10760, #5551, #299, .T. ) ;
#12643 = CARTESIAN_POINT ( 'NONE',  ( 1.749999999999998002, 0.000000000000000000, 0.000000000000000000 ) ) ;
#12644 = CARTESIAN_POINT ( 'NONE',  ( 2.789999999999999147, 0.000000000000000000, 0.000000000000000000 ) ) ;
#12645 = CARTESIAN_POINT ( 'NONE',  ( 2.604434404052931473, -17.45907811351440841, -19.17825124759797006 ) ) ;
#12646 = DIRECTION ( 'NONE',  ( 1.000000000000000000, 0.000000000000000000, 0.000000000000000000 ) ) ;
#12647 = ORIENTED_EDGE ( 'NONE', *, *, #14558, .F. ) ;
#12648 = CARTESIAN_POINT ( 'NONE',  ( -9.403944755730119454, -4.794738323547945491, 12.00000000000000000 ) ) ;
#12649 = CARTESIAN_POINT ( 'NONE',  ( 14.40394475573011945, -10.79473832354794460, 5.500000000000001776 ) ) ;
#12650 = CARTESIAN_POINT ( 'NONE',  ( 2.718184757033984766, -16.91181672897746324, 18.89296398180185932 ) ) ;
#12651 = ADVANCED_FACE ( 'NONE', ( #14790 ), #7569, .F. ) ;
#12652 = EDGE_CURVE ( 'NONE', #12037, #12877, #4595, .T. ) ;
#12653 = VERTEX_POINT ( 'NONE', #6565 ) ;
#12654 = DIRECTION ( 'NONE',  ( 1.000000000000000000, 0.000000000000000000, 0.000000000000000000 ) ) ;
#12655 = CARTESIAN_POINT ( 'NONE',  ( -0.1085714285714285687, -3.798448662927795372, 0.000000000000000000 ) ) ;
#12656 = ORIENTED_EDGE ( 'NONE', *, *, #11905, .T. ) ;
#12657 = VERTEX_POINT ( 'NONE', #5426 ) ;
#12658 = CARTESIAN_POINT ( 'NONE',  ( -1.250000000000001110, 0.000000000000000000, 0.000000000000000000 ) ) ;
#12659 = CIRCLE ( 'NONE', #11444, 3.000000000000002665 ) ;
#12660 = CARTESIAN_POINT ( 'NONE',  ( -10.00000000000000000, 0.000000000000000000, 0.000000000000000000 ) ) ;
#12661 = ORIENTED_EDGE ( 'NONE', *, *, #11081, .F. ) ;
#12662 = DIRECTION ( 'NONE',  ( 0.000000000000000000, 0.9510565162951498674, 0.3090169943749583870 ) ) ;
#12663 = CARTESIAN_POINT ( 'NONE',  ( 0.000000000000000000, -5.535312321042547445, -23.48180575137738302 ) ) ;
#12664 = DIRECTION ( 'NONE',  ( 0.1305261922200521840, -0.9914448613738103822, 0.000000000000000000 ) ) ;
#12665 = CARTESIAN_POINT ( 'NONE',  ( 2.789999999999999147, -12.98979500319697955, 5.249430348645709010 ) ) ;
#12666 = CYLINDRICAL_SURFACE ( 'NONE', #10851, 8.400000000000000355 ) ;
#12667 = EDGE_CURVE ( 'NONE', #10918, #12266, #13161, .T. ) ;
#12668 = EDGE_CURVE ( 'NONE', #14957, #1993, #13627, .T. ) ;
#12669 = VERTEX_POINT ( 'NONE', #11319 ) ;
#12670 = AXIS2_PLACEMENT_3D ( 'NONE', #51, #8363, #13042 ) ;
#12671 = B_SPLINE_CURVE_WITH_KNOTS ( 'NONE', 3,
 ( #15200, #3721, #24, #2569 ),
 .UNSPECIFIED., .F., .F.,
 ( 4, 4 ),
 ( 0.005258120783916792398, 0.005948386350302926374 ),
 .UNSPECIFIED. ) ;
#12672 = CARTESIAN_POINT ( 'NONE',  ( 0.000000000000000000, 15.04425356660760293, 20.70663861606276868 ) ) ;
#12673 = CARTESIAN_POINT ( 'NONE',  ( 2.789999999999999147, 2.311161484776756758, -14.46287784598614756 ) ) ;
#12674 = EDGE_CURVE ( 'NONE', #13716, #4803, #8500, .T. ) ;
#12675 = VERTEX_POINT ( 'NONE', #11471 ) ;
#12676 = AXIS2_PLACEMENT_3D ( 'NONE', #2114, #13867, #9041 ) ;
#12677 =( NAMED_UNIT ( * ) PLANE_ANGLE_UNIT ( ) SI_UNIT ( $, .RADIAN. ) );
#12678 = ORIENTED_EDGE ( 'NONE', *, *, #8349, .T. ) ;
#12679 = ORIENTED_EDGE ( 'NONE', *, *, #7030, .T. ) ;
#12680 = ORIENTED_EDGE ( 'NONE', *, *, #29, .T. ) ;
#12681 = DIRECTION ( 'NONE',  ( -1.000000000000000000, -0.000000000000000000, -0.000000000000000000 ) ) ;
#12682 = LINE ( 'NONE', #6998, #6105 ) ;
#12683 = EDGE_CURVE ( 'NONE', #14255, #9774, #7009, .T. ) ;
#12684 = CARTESIAN_POINT ( 'NONE',  ( 2.582362639458679610, -5.278564329440899705, -14.94126095370966567 ) ) ;
#12685 = SHAPE_REPRESENTATION ( 'MAS-167', ( #7212, #11129, #6474, #6716, #2544, #15076, #824, #3550, #4762, #4521, #10640, #13336, #7943, #8214, #9406, #8703, #7493, #9444, #2787, #10188, #12138, #13081, #14619 ), #5264 ) ;
#12686 = CARTESIAN_POINT ( 'NONE',  ( 0.007349557670559579703, -9.045126717605857181, 11.23191127083860508 ) ) ;
#12687 = VECTOR ( 'NONE', #14045, 1000.000000000000000 ) ;
#12688 = ORIENTED_EDGE ( 'NONE', *, *, #13560, .T. ) ;
#12689 = AXIS2_PLACEMENT_3D ( 'NONE', #8750, #7539, #7680 ) ;
#12690 = CARTESIAN_POINT ( 'NONE',  ( 67.23404255319148604, 28.93147646537027384, 7.000000000000000000 ) ) ;
#12691 = CARTESIAN_POINT ( 'NONE',  ( 1.039999999999996483, 4.147968289691283950, 27.76164181293052735 ) ) ;
#12692 = ADVANCED_FACE ( 'NONE', ( #11544, #1095 ), #6940, .T. ) ;
#12693 = DIRECTION ( 'NONE',  ( 0.000000000000000000, 0.000000000000000000, -1.000000000000000000 ) ) ;
#12694 = VERTEX_POINT ( 'NONE', #4650 ) ;
#12695 = CIRCLE ( 'NONE', #8008, 4.999999999999997335 ) ;
#12696 = FACE_OUTER_BOUND ( 'NONE', #1533, .T. ) ;
#12697 = CARTESIAN_POINT ( 'NONE',  ( 0.000000000000000000, 0.000000000000000000, 6.000000000000000000 ) ) ;
#12698 = CIRCLE ( 'NONE', #7319, 2.524999999999998579 ) ;
#12699 = VERTEX_POINT ( 'NONE', #8097 ) ;
#12700 = VERTEX_POINT ( 'NONE', #5793 ) ;
#12701 = AXIS2_PLACEMENT_3D ( 'NONE', #12311, #11085, #6637 ) ;
#12702 = CARTESIAN_POINT ( 'NONE',  ( 91.46153288930040048, 16.46030115554384565, 4.000000000000000000 ) ) ;
#12703 = EDGE_LOOP ( 'NONE', ( #14914, #9315, #3201, #12459 ) ) ;
#12704 = CARTESIAN_POINT ( 'NONE',  ( 2.582362639458678277, 14.94126095370968166, -5.278564329440845526 ) ) ;
#12705 = AXIS2_PLACEMENT_3D ( 'NONE', #7930, #9088, #13772 ) ;
#12706 = DIRECTION ( 'NONE',  ( 0.9021244663126475327, 0.4314758942051350465, -1.141265444721583757E-16 ) ) ;
#12707 = ADVANCED_FACE ( 'NONE', ( #3408 ), #12770, .F. ) ;
#12708 = LINE ( 'NONE', #10401, #2076 ) ;
#12709 = CARTESIAN_POINT ( 'NONE',  ( 18.71314632718394222, -23.25585687728512241, -2.000000000000000000 ) ) ;
#12710 = TOROIDAL_SURFACE ( 'NONE', #4139, 4.100000000000000533, 0.1000000000000001582 ) ;
#12711 = VERTEX_POINT ( 'NONE', #14007 ) ;
#12712 = SURFACE_SIDE_STYLE ('',( #12500 ) ) ;
#12713 = CARTESIAN_POINT ( 'NONE',  ( 0.4522159373304727170, 3.429166897524654534, -16.32199768300075249 ) ) ;
#12714 = VERTEX_POINT ( 'NONE', #4565 ) ;
#12715 = EDGE_LOOP ( 'NONE', ( #5971, #1094 ) ) ;
#12716 = CYLINDRICAL_SURFACE ( 'NONE', #11968, 6.000000000000005329 ) ;
#12717 = DIRECTION ( 'NONE',  ( 0.000000000000000000, 0.000000000000000000, 1.000000000000000000 ) ) ;
#12718 = CARTESIAN_POINT ( 'NONE',  ( 1.150000000000001688, 0.000000000000000000, -6.000000000000000888 ) ) ;
#12719 = FACE_OUTER_BOUND ( 'NONE', #10541, .T. ) ;
#12720 = AXIS2_PLACEMENT_3D ( 'NONE', #10202, #13741, #12579 ) ;
#12721 = CARTESIAN_POINT ( 'NONE',  ( 0.02531912748256377743, 14.46287784598617421, -2.311161484776606212 ) ) ;
#12722 = CARTESIAN_POINT ( 'NONE',  ( 1.749999999999999778, 4.458161950358502601, 17.39253030560843172 ) ) ;
#12723 = ADVANCED_FACE ( 'NONE', ( #7873 ), #11389, .T. ) ;
#12724 = ORIENTED_EDGE ( 'NONE', *, *, #211, .T. ) ;
#12725 = DIRECTION ( 'NONE',  ( -1.000000000000000000, 0.000000000000000000, -0.000000000000000000 ) ) ;
#12726 = LINE ( 'NONE', #2356, #1524 ) ;
#12727 = B_SPLINE_CURVE_WITH_KNOTS ( 'NONE', 3,
 ( #152, #8458, #10700, #6012, #13234, #4873, #5108, #1398 ),
 .UNSPECIFIED., .F., .F.,
 ( 4, 2, 2, 4 ),
 ( 4.663089342034313692E-07, 0.001898630032275744253, 0.002847711893946512033, 0.003796793755617279813 ),
 .UNSPECIFIED. ) ;
#12728 = FACE_OUTER_BOUND ( 'NONE', #3565, .T. ) ;
#12729 = CARTESIAN_POINT ( 'NONE',  ( 2.789999999999999147, -5.249430348645846678, 12.98979500319692448 ) ) ;
#12730 = ORIENTED_EDGE ( 'NONE', *, *, #2301, .F. ) ;
#12731 = EDGE_CURVE ( 'NONE', #14436, #2991, #4075, .T. ) ;
#12732 = CIRCLE ( 'NONE', #10536, 2.524999999999999467 ) ;
#12733 = DIRECTION ( 'NONE',  ( -1.000000000000000000, -0.000000000000000000, -0.000000000000000000 ) ) ;
#12734 = CARTESIAN_POINT ( 'NONE',  ( 2.718131847775120402, 5.344160105509049963, -24.78765742476133482 ) ) ;
#12735 = ORIENTED_EDGE ( 'NONE', *, *, #12642, .T. ) ;
#12736 = ORIENTED_EDGE ( 'NONE', *, *, #914, .F. ) ;
#12737 = CARTESIAN_POINT ( 'NONE',  ( 1.749999999999998002, -25.12109765559663188, 12.52377138324213668 ) ) ;
#12738 = CARTESIAN_POINT ( 'NONE',  ( 1.749999999999998002, -19.67366047555515252, -20.02152543075368030 ) ) ;
#12739 = ORIENTED_EDGE ( 'NONE', *, *, #4587, .F. ) ;
#12740 = CARTESIAN_POINT ( 'NONE',  ( 2.789999999999999147, 0.000000000000000000, 0.000000000000000000 ) ) ;
#12741 = CARTESIAN_POINT ( 'NONE',  ( 2.765633920072238627, -21.30679549418621832, -12.59161484032935618 ) ) ;
#12742 = CARTESIAN_POINT ( 'NONE',  ( 0.02531912748464674665, 5.229914364928542447, -13.68080036884343009 ) ) ;
#12743 = EDGE_CURVE ( 'NONE', #12163, #1742, #6709, .T. ) ;
#12744 = EDGE_CURVE ( 'NONE', #10607, #6338, #8970, .T. ) ;
#12745 = LINE ( 'NONE', #6913, #1719 ) ;
#12746 = PLANE ( 'NONE',  #4902 ) ;
#12747 = VECTOR ( 'NONE', #13597, 1000.000000000000000 ) ;
#12748 = ORIENTED_EDGE ( 'NONE', *, *, #9245, .F. ) ;
#12749 = B_SPLINE_CURVE_WITH_KNOTS ( 'NONE', 3,
 ( #2596, #9888, #11961, #14587, #12036, #11880, #504, #1448 ),
 .UNSPECIFIED., .F., .F.,
 ( 4, 2, 2, 4 ),
 ( 1.984117563342667082E-07, 0.001895214258086359458, 0.002842722181251369599, 0.003790230104416379524 ),
 .UNSPECIFIED. ) ;
#12750 = LINE ( 'NONE', #1072, #3833 ) ;
#12751 = CARTESIAN_POINT ( 'NONE',  ( 2.790000000000000036, 23.69843731927168662, 5.456805104201184697 ) ) ;
#12752 = ORIENTED_EDGE ( 'NONE', *, *, #9953, .T. ) ;
#12753 = SURFACE_SIDE_STYLE ('',( #8079 ) ) ;
#12754 = ORIENTED_EDGE ( 'NONE', *, *, #8548, .T. ) ;
#12755 = VERTEX_POINT ( 'NONE', #9021 ) ;
#12756 = ORIENTED_EDGE ( 'NONE', *, *, #2032, .F. ) ;
#12757 = DIRECTION ( 'NONE',  ( 0.000000000000000000, 0.000000000000000000, 1.000000000000000000 ) ) ;
#12758 = EDGE_CURVE ( 'NONE', #7028, #1566, #10363, .T. ) ;
#12759 = CARTESIAN_POINT ( 'NONE',  ( 8.000000000000000000, 0.000000000000000000, 0.000000000000000000 ) ) ;
#12760 = DIRECTION ( 'NONE',  ( 0.000000000000000000, 0.000000000000000000, -1.000000000000000000 ) ) ;
#12761 = DIRECTION ( 'NONE',  ( 0.000000000000000000, 0.000000000000000000, 1.000000000000000000 ) ) ;
#12762 = EDGE_CURVE ( 'NONE', #6646, #12118, #8229, .T. ) ;
#12763 = UNCERTAINTY_MEASURE_WITH_UNIT (LENGTH_MEASURE( 1.000000000000000082E-05 ), #13444, 'distance_accuracy_value', 'NONE');
#12764 = CARTESIAN_POINT ( 'NONE',  ( 2.765633920072238627, -21.30679549418621832, -12.59161484032935618 ) ) ;
#12765 = ORIENTED_EDGE ( 'NONE', *, *, #6777, .T. ) ;
#12766 = CARTESIAN_POINT ( 'NONE',  ( 1.749999999999998002, -4.633866840648726004, -27.68468304288263582 ) ) ;
#12767 = EDGE_CURVE ( 'NONE', #13926, #7258, #10694, .T. ) ;
#12768 = CARTESIAN_POINT ( 'NONE',  ( 84.00000000000000000, 0.000000000000000000, 6.000000000000000000 ) ) ;
#12769 = VERTEX_POINT ( 'NONE', #3474 ) ;
#12770 = CYLINDRICAL_SURFACE ( 'NONE', #14870, 9.999999999999994671 ) ;
#12771 = PRODUCT_DEFINITION_SHAPE ( 'NONE', 'NONE',  #15223 ) ;
#12772 = DIRECTION ( 'NONE',  ( 1.000000000000000000, 0.000000000000000000, 0.000000000000000000 ) ) ;
#12773 = EDGE_LOOP ( 'NONE', ( #12536, #5531, #10780, #9714 ) ) ;
#12774 = VERTEX_POINT ( 'NONE', #8162 ) ;
#12775 = DIRECTION ( 'NONE',  ( 0.000000000000000000, 0.000000000000000000, 1.000000000000000000 ) ) ;
#12776 = ORIENTED_EDGE ( 'NONE', *, *, #13416, .F. ) ;
#12777 = FACE_OUTER_BOUND ( 'NONE', #10586, .T. ) ;
#12778 = CARTESIAN_POINT ( 'NONE',  ( 2.764680872513205934, -11.36963888406694068, 9.232963481057725019 ) ) ;
#12779 = DIRECTION ( 'NONE',  ( 0.02857142857142857401, 0.9995917534020515305, -0.000000000000000000 ) ) ;
#12780 = DIRECTION ( 'NONE',  ( 0.000000000000000000, 0.000000000000000000, 1.000000000000000000 ) ) ;
#12781 = ORIENTED_EDGE ( 'NONE', *, *, #2644, .F. ) ;
#12782 = DIRECTION ( 'NONE',  ( 1.000000000000000000, 0.000000000000000000, 0.000000000000000000 ) ) ;
#12783 = CARTESIAN_POINT ( 'NONE',  ( 2.257825477245765988, -19.66801664102690239, -18.57583492944443293 ) ) ;
#12784 = ORIENTED_EDGE ( 'NONE', *, *, #6937, .F. ) ;
#12785 = ORIENTED_EDGE ( 'NONE', *, *, #4425, .T. ) ;
#12786 = CARTESIAN_POINT ( 'NONE',  ( 0.006974663525957706944, 21.08118142846903353, 12.53640742967760602 ) ) ;
#12787 = DIRECTION ( 'NONE',  ( 0.000000000000000000, 0.000000000000000000, 1.000000000000000000 ) ) ;
#12788 = DIRECTION ( 'NONE',  ( 0.7573544145849105957, -0.6530040510661073716, -2.081668171172162967E-17 ) ) ;
#12789 = DIRECTION ( 'NONE',  ( 1.000000000000000000, 1.445602896647338424E-16, 0.000000000000000000 ) ) ;
#12790 = CARTESIAN_POINT ( 'NONE',  ( -6.138153946363927094E-14, 14.05326139264726315, -2.096282088614805250 ) ) ;
#12791 = ADVANCED_FACE ( 'NONE', ( #14953 ), #7938, .T. ) ;
#12792 = DIRECTION ( 'NONE',  ( 1.000000000000000000, 0.000000000000000000, -0.000000000000000000 ) ) ;
#12793 = ORIENTED_EDGE ( 'NONE', *, *, #15179, .T. ) ;
#12794 = CARTESIAN_POINT ( 'NONE',  ( -10.00000000000000000, 0.000000000000000000, 0.000000000000000000 ) ) ;
#12795 = CARTESIAN_POINT ( 'NONE',  ( 111.6227766016837961, 7.610970684806392799E-15, 3.000000000000002665 ) ) ;
#12796 = CARTESIAN_POINT ( 'NONE',  ( 0.000000000000000000, 15.04425356660790136, -18.18163861606255338 ) ) ;
#12797 = CARTESIAN_POINT ( 'NONE',  ( 2.789999999999999147, 3.120158876139031534, 14.59528211760003558 ) ) ;
#12798 = VECTOR ( 'NONE', #755, 1000.000000000000000 ) ;
#12799 = ORIENTED_EDGE ( 'NONE', *, *, #2070, .F. ) ;
#12800 = B_SPLINE_CURVE_WITH_KNOTS ( 'NONE', 3,
 ( #5803, #4658, #9335, #14016 ),
 .UNSPECIFIED., .F., .F.,
 ( 4, 4 ),
 ( 2.135345996173299606E-07, 0.0006888010880210790939 ),
 .UNSPECIFIED. ) ;
#12801 = EDGE_CURVE ( 'NONE', #6027, #12188, #615, .T. ) ;
#12802 = DIRECTION ( 'NONE',  ( 0.000000000000000000, 0.000000000000000000, 1.000000000000000000 ) ) ;
#12803 = CARTESIAN_POINT ( 'NONE',  ( 0.1438988480186108865, -14.59528211759996630, 5.279841123860814278 ) ) ;
#12804 = ORIENTED_EDGE ( 'NONE', *, *, #4968, .F. ) ;
#12805 = LINE ( 'NONE', #11736, #13177 ) ;
#12806 = CARTESIAN_POINT ( 'NONE',  ( 56.98919079003883326, 3.953582723775848962, 6.000000000000000000 ) ) ;
#12807 = ADVANCED_FACE ( 'NONE', ( #12696 ), #6868, .T. ) ;
#12808 = DIRECTION ( 'NONE',  ( 1.000000000000000000, 0.000000000000000000, -0.000000000000000000 ) ) ;
#12809 = CARTESIAN_POINT ( 'NONE',  ( -1.149999999999998135, 4.898587196589412829E-16, 4.000000000000000000 ) ) ;
#12810 = CARTESIAN_POINT ( 'NONE',  ( 2.789999999999999147, 20.62201879784931435, -12.52067188844328882 ) ) ;
#12811 = AXIS2_PLACEMENT_3D ( 'NONE', #919, #4537, #5403 ) ;
#12812 = CIRCLE ( 'NONE', #5480, 2.524999999999996358 ) ;
#12813 = EDGE_CURVE ( 'NONE', #14991, #1378, #10926, .T. ) ;
#12814 = CARTESIAN_POINT ( 'NONE',  ( -14.40394475573012301, -4.794738323547945491, 16.99999999999999645 ) ) ;
#12815 = DIRECTION ( 'NONE',  ( 0.7573544145849105957, -0.6530040510661073716, -2.081668171172162967E-17 ) ) ;
#12816 = VERTEX_POINT ( 'NONE', #14159 ) ;
#12817 = CARTESIAN_POINT ( 'NONE',  ( 0.02436607992775978102, -12.59161484032896361, -21.30679549418645280 ) ) ;
#12818 = CARTESIAN_POINT ( 'NONE',  ( 18.38434835257323030, -21.28306902962084024, 4.000000000000000000 ) ) ;
#12819 = VERTEX_POINT ( 'NONE', #8457 ) ;
#12820 = ADVANCED_FACE ( 'NONE', ( #11768 ), #305, .T. ) ;
#12821 = CIRCLE ( 'NONE', #4995, 4.000000000000000000 ) ;
#12822 = ORIENTED_EDGE ( 'NONE', *, *, #13987, .F. ) ;
#12823 = ORIENTED_EDGE ( 'NONE', *, *, #8887, .T. ) ;
#12824 = ORIENTED_EDGE ( 'NONE', *, *, #1732, .F. ) ;
#12825 = DIRECTION ( 'NONE',  ( 0.000000000000000000, 0.000000000000000000, -1.000000000000000000 ) ) ;
#12826 = FACE_OUTER_BOUND ( 'NONE', #3439, .T. ) ;
#12827 = CARTESIAN_POINT ( 'NONE',  ( 2.765633920072235075, -12.59161484032896361, -21.30679549418645280 ) ) ;
#12828 = CARTESIAN_POINT ( 'NONE',  ( 1.824075699840007170, -24.74770846292491910, 12.96726489871182153 ) ) ;
#12829 = ADVANCED_FACE ( 'NONE', ( #14076 ), #14238, .F. ) ;
#12830 = DIRECTION ( 'NONE',  ( -1.000000000000000000, -0.000000000000000000, -0.000000000000000000 ) ) ;
#12831 = VERTEX_POINT ( 'NONE', #10778 ) ;
#12832 = LINE ( 'NONE', #11765, #14405 ) ;
#12833 = ADVANCED_FACE ( 'NONE', ( #10623 ), #13145, .F. ) ;
#12834 = EDGE_CURVE ( 'NONE', #3292, #11269, #5938, .T. ) ;
#12835 = EDGE_CURVE ( 'NONE', #11615, #14392, #7163, .T. ) ;
#12836 = EDGE_LOOP ( 'NONE', ( #7429, #2969, #2338, #4892 ) ) ;
#12837 = DIRECTION ( 'NONE',  ( -1.000000000000000000, 0.000000000000000000, 0.000000000000000000 ) ) ;
#12838 = DIRECTION ( 'NONE',  ( 0.000000000000000000, 0.000000000000000000, 1.000000000000000000 ) ) ;
#12839 = ORIENTED_EDGE ( 'NONE', *, *, #14756, .T. ) ;
#12840 = ORIENTED_EDGE ( 'NONE', *, *, #1370, .T. ) ;
#12841 = DIRECTION ( 'NONE',  ( 0.000000000000000000, 0.000000000000000000, 1.000000000000000000 ) ) ;
#12842 = ORIENTED_EDGE ( 'NONE', *, *, #8072, .T. ) ;
#12843 = DIRECTION ( 'NONE',  ( 0.000000000000000000, 0.000000000000000000, -1.000000000000000000 ) ) ;
#12844 = FACE_OUTER_BOUND ( 'NONE', #6795, .T. ) ;
#12845 = EDGE_CURVE ( 'NONE', #484, #12141, #12884, .T. ) ;
#12846 = CYLINDRICAL_SURFACE ( 'NONE', #576, 28.06981291497571362 ) ;
#12847 = CARTESIAN_POINT ( 'NONE',  ( -10.00000000000000000, -2.081668171172168513E-15, 7.000000000000000000 ) ) ;
#12848 = AXIS2_PLACEMENT_3D ( 'NONE', #2645, #10789, #165 ) ;
#12849 = VECTOR ( 'NONE', #13948, 1000.000000000000000 ) ;
#12850 = ORIENTED_EDGE ( 'NONE', *, *, #2847, .F. ) ;
#12851 = CARTESIAN_POINT ( 'NONE',  ( 0.1374368770859597522, -4.808326913195983821, -0.8000000000000000444 ) ) ;
#12852 = EDGE_CURVE ( 'NONE', #8452, #1420, #9220, .T. ) ;
#12853 = CARTESIAN_POINT ( 'NONE',  ( 2.718184757033982102, -18.89296398180179537, -16.91181672897754495 ) ) ;
#12854 = EDGE_LOOP ( 'NONE', ( #10703, #14318, #9059, #13606 ) ) ;
#12855 = EDGE_LOOP ( 'NONE', ( #14828, #10228, #8829, #8318 ) ) ;
#12856 = DIRECTION ( 'NONE',  ( -0.000000000000000000, -1.000000000000000000, -0.000000000000000000 ) ) ;
#12858 = LINE ( 'NONE', #10502, #12479 ) ;
#12857 = CIRCLE ( 'NONE', #8943, 24.12539914357697768 ) ;
#12859 = ADVANCED_FACE ( 'NONE', ( #11994 ), #229, .T. ) ;
#12860 = VECTOR ( 'NONE', #2997, 1000.000000000000000 ) ;
#12861 = DIRECTION ( 'NONE',  ( -1.000000000000000000, 0.000000000000000000, -0.000000000000000000 ) ) ;
#12862 = VECTOR ( 'NONE', #7068, 1000.000000000000114 ) ;
#12863 = FACE_OUTER_BOUND ( 'NONE', #8265, .T. ) ;
#12864 = DIRECTION ( 'NONE',  ( 1.000000000000000000, 0.000000000000000000, 0.000000000000000000 ) ) ;
#12865 = DIRECTION ( 'NONE',  ( 0.1643989873053574580, -0.9863939238321436376, 0.000000000000000000 ) ) ;
#12866 = ORIENTED_EDGE ( 'NONE', *, *, #9250, .F. ) ;
#12867 = CARTESIAN_POINT ( 'NONE',  ( 2.789999999999999147, 24.04302995059966364, 1.991882183130384121 ) ) ;
#12868 = CARTESIAN_POINT ( 'NONE',  ( 0.1882239034349757756, -12.84621645676860702, 22.54313264455009147 ) ) ;
#12869 = CARTESIAN_POINT ( 'NONE',  ( 0.007349505829628562997, 5.204557061642287152, 13.44926448535267838 ) ) ;
#12870 = AXIS2_PLACEMENT_3D ( 'NONE', #1983, #5520, #9198 ) ;
#12871 = DIRECTION ( 'NONE',  ( -1.000000000000000000, 0.000000000000000000, 0.000000000000000000 ) ) ;
#12872 = VERTEX_POINT ( 'NONE', #1479 ) ;
#12873 = AXIS2_PLACEMENT_3D ( 'NONE', #9327, #11995, #14077 ) ;
#12874 = ORIENTED_EDGE ( 'NONE', *, *, #12683, .T. ) ;
#12875 = EDGE_CURVE ( 'NONE', #5202, #3390, #13094, .T. ) ;
#12876 = FACE_OUTER_BOUND ( 'NONE', #6175, .T. ) ;
#12877 = VERTEX_POINT ( 'NONE', #1174 ) ;
#12878 = CARTESIAN_POINT ( 'NONE',  ( 2.236220312281013811, 12.52687487503435193, -11.41743294611062254 ) ) ;
#12879 = LINE ( 'NONE', #9587, #1418 ) ;
#12880 = DIRECTION ( 'NONE',  ( 1.445602896647338917E-16, -1.000000000000000000, -0.000000000000000000 ) ) ;
#12881 = DIRECTION ( 'NONE',  ( 0.000000000000000000, 0.000000000000000000, 1.000000000000000000 ) ) ;
#12882 = CARTESIAN_POINT ( 'NONE',  ( 0.006974657972265005043, 23.92335783895637746, 5.408388659524176134 ) ) ;
#12883 = AXIS2_PLACEMENT_3D ( 'NONE', #13786, #7942, #13635 ) ;
#12884 = CIRCLE ( 'NONE', #12403, 2.524999999999999467 ) ;
#12885 = DIRECTION ( 'NONE',  ( 0.000000000000000000, 0.000000000000000000, 1.000000000000000000 ) ) ;
#12886 = DIRECTION ( 'NONE',  ( -1.000000000000000000, -0.000000000000000000, -0.000000000000000000 ) ) ;
#12887 = ORIENTED_EDGE ( 'NONE', *, *, #14741, .F. ) ;
#12888 = PRODUCT_DEFINITION_SHAPE ( 'NONE', 'NONE',  #15225 ) ;
#12889 = CARTESIAN_POINT ( 'NONE',  ( 0.000000000000000000, 0.000000000000000000, 0.000000000000000000 ) ) ;
#12890 = EDGE_CURVE ( 'NONE', #5429, #13724, #3810, .T. ) ;
#12891 = ORIENTED_EDGE ( 'NONE', *, *, #113, .F. ) ;
#12892 =( NAMED_UNIT ( * ) PLANE_ANGLE_UNIT ( ) SI_UNIT ( $, .RADIAN. ) );
#12893 = VERTEX_POINT ( 'NONE', #10553 ) ;
#12894 = ORIENTED_EDGE ( 'NONE', *, *, #8230, .F. ) ;
#12895 = ORIENTED_EDGE ( 'NONE', *, *, #3365, .F. ) ;
#12896 = CARTESIAN_POINT ( 'NONE',  ( 0.000000000000000000, 0.000000000000000000, 3.000000000000000000 ) ) ;
#12897 = CARTESIAN_POINT ( 'NONE',  ( 2.789999999999999147, -23.48180575137734039, 5.535312321042630934 ) ) ;
#12898 = CARTESIAN_POINT ( 'NONE',  ( 60.64109936584995353, 31.48746944824151583, 2.000000000000000000 ) ) ;
#12899 = PLANE ( 'NONE',  #4036 ) ;
#12900 = VECTOR ( 'NONE', #6537, 1000.000000000000000 ) ;
#12901 = DIRECTION ( 'NONE',  ( -0.9148936170212770280, -0.4036950204470263204, 0.000000000000000000 ) ) ;
#12902 = B_SPLINE_CURVE_WITH_KNOTS ( 'NONE', 3,
 ( #13053, #3468, #8373, #10465 ),
 .UNSPECIFIED., .F., .F.,
 ( 4, 4 ),
 ( 0.005258139959819239928, 0.005948405594583421920 ),
 .UNSPECIFIED. ) ;
#12903 = VECTOR ( 'NONE', #4068, 1000.000000000000000 ) ;
#12904 = ORIENTED_EDGE ( 'NONE', *, *, #10774, .T. ) ;
#12905 = CARTESIAN_POINT ( 'NONE',  ( 2.789999999999999147, -24.04302995059966719, 1.991882183130210482 ) ) ;
#12906 = B_SPLINE_CURVE_WITH_KNOTS ( 'NONE', 3,
 ( #10212, #11511, #14831, #7841 ),
 .UNSPECIFIED., .F., .F.,
 ( 4, 4 ),
 ( 0.005540500595652342840, 0.005814376014856851432 ),
 .UNSPECIFIED. ) ;
#12907 = AXIS2_PLACEMENT_3D ( 'NONE', #10585, #34, #12951 ) ;
#12908 = AXIS2_PLACEMENT_3D ( 'NONE', #2399, #10619, #4865 ) ;
#12909 = EDGE_CURVE ( 'NONE', #8554, #12141, #119, .T. ) ;
#12910 = ORIENTED_EDGE ( 'NONE', *, *, #11338, .F. ) ;
#12911 = DIRECTION ( 'NONE',  ( 1.000000000000000000, 0.000000000000000000, 0.000000000000000000 ) ) ;
#12912 = CARTESIAN_POINT ( 'NONE',  ( 2.789999999999999147, 2.311161484776556030, 14.46287784598618309 ) ) ;
#12913 = VERTEX_POINT ( 'NONE', #3695 ) ;
#12914 = EDGE_LOOP ( 'NONE', ( #9081, #13008 ) ) ;
#12915 = CIRCLE ( 'NONE', #403, 2.447112362156698140 ) ;
#12916 = PLANE ( 'NONE',  #2342 ) ;
#12917 = PRODUCT_DEFINITION ( 'UNKNOWN', '', #4021, #7630 ) ;
#12918 = EDGE_CURVE ( 'NONE', #13931, #6657, #2101, .T. ) ;
#12919 = EDGE_LOOP ( 'NONE', ( #1692, #8415, #15115, #7375 ) ) ;
#12920 = CIRCLE ( 'NONE', #14418, 2.524999999999995914 ) ;
#12921 = EDGE_CURVE ( 'NONE', #7248, #241, #13872, .T. ) ;
#12922 = CARTESIAN_POINT ( 'NONE',  ( 1.039999999999999147, 12.52377138324259676, -25.12109765559640095 ) ) ;
#12923 = CARTESIAN_POINT ( 'NONE',  ( -14.40394475573011945, -10.79473832354794460, -5.000000000000000000 ) ) ;
#12924 = CARTESIAN_POINT ( 'NONE',  ( 1.039999999999998259, 12.52377138324223615, 25.12109765559657859 ) ) ;
#12925 = LINE ( 'NONE', #14173, #12849 ) ;
#12926 = CIRCLE ( 'NONE', #10248, 28.06981291497571007 ) ;
#12927 = ORIENTED_EDGE ( 'NONE', *, *, #9459, .F. ) ;
#12928 = AXIS2_PLACEMENT_3D ( 'NONE', #13405, #14502, #6117 ) ;
#12929 = FACE_OUTER_BOUND ( 'NONE', #11144, .T. ) ;
#12930 = CARTESIAN_POINT ( 'NONE',  ( 1.666666666666673624, 0.000000000000000000, 6.000000000000000000 ) ) ;
#12931 = CIRCLE ( 'NONE', #10743, 28.06981291497571362 ) ;
#12932 = VECTOR ( 'NONE', #13721, 1000.000000000000000 ) ;
#12933 = EDGE_LOOP ( 'NONE', ( #3193, #2744, #8979, #11197, #15126, #12578 ) ) ;
#12934 = ORIENTED_EDGE ( 'NONE', *, *, #15017, .T. ) ;
#12935 = ADVANCED_FACE ( 'NONE', ( #14312 ), #8315, .F. ) ;
#12936 = CARTESIAN_POINT ( 'NONE',  ( -14.40394475573012301, -4.794738323547945491, 13.99999999999999645 ) ) ;
#12937 = CARTESIAN_POINT ( 'NONE',  ( 2.788130827028544534, 20.90869469097885158, -12.51925356660739297 ) ) ;
#12938 = EDGE_CURVE ( 'NONE', #1316, #3142, #10559, .T. ) ;
#12939 = VECTOR ( 'NONE', #14099, 1000.000000000000000 ) ;
#12940 = CYLINDRICAL_SURFACE ( 'NONE', #8044, 8.400000000000000355 ) ;
#12941 = CYLINDRICAL_SURFACE ( 'NONE', #12625, 28.06981291497571362 ) ;
#12942 = CYLINDRICAL_SURFACE ( 'NONE', #7089, 2.524999999999995914 ) ;
#12943 = EDGE_CURVE ( 'NONE', #8603, #2360, #8923, .T. ) ;
#12944 = AXIS2_PLACEMENT_3D ( 'NONE', #14885, #4508, #3134 ) ;
#12945 = AXIS2_PLACEMENT_3D ( 'NONE', #8362, #124, #1015 ) ;
#12946 = CARTESIAN_POINT ( 'NONE',  ( 2.236220346785028568, 3.624349476775199808, 16.55730827443882802 ) ) ;
#12947 = ORIENTED_EDGE ( 'NONE', *, *, #13073, .T. ) ;
#12948 = CARTESIAN_POINT ( 'NONE',  ( 1.000000000000000000, -4.808326913195983821, -0.8000000000000000444 ) ) ;
#12949 = CARTESIAN_POINT ( 'NONE',  ( 0.02436607992775934733, -2.336989772644440855, 24.63872515616082026 ) ) ;
#12950 = DIRECTION ( 'NONE',  ( -1.000000000000000000, -0.000000000000000000, -0.000000000000000000 ) ) ;
#12951 = DIRECTION ( 'NONE',  ( 0.000000000000000000, 0.000000000000000000, 1.000000000000000000 ) ) ;
#12952 = EDGE_CURVE ( 'NONE', #5949, #13989, #9960, .T. ) ;
#12953 = ORIENTED_EDGE ( 'NONE', *, *, #1791, .F. ) ;
#12954 = AXIS2_PLACEMENT_3D ( 'NONE', #14605, #10361, #13823 ) ;
#12955 = ORIENTED_EDGE ( 'NONE', *, *, #3517, .F. ) ;
#12956 = CARTESIAN_POINT ( 'NONE',  ( 0.000000000000000000, 7.739906618939895289, -13.40591150984218416 ) ) ;
#12957 = ORIENTED_EDGE ( 'NONE', *, *, #1126, .F. ) ;
#12958 = AXIS2_PLACEMENT_3D ( 'NONE', #11280, #14981, #7745 ) ;
#12959 = CARTESIAN_POINT ( 'NONE',  ( 0.2818302809372421058, 10.58084377126623288, 12.18203740414270619 ) ) ;
#12960 = CARTESIAN_POINT ( 'NONE',  ( 59.05334708265789345, 38.04890259842303379, 4.000000000000000000 ) ) ;
#12961 = B_SPLINE_CURVE_WITH_KNOTS ( 'NONE', 3,
 ( #1948, #6633, #11152, #11312, #6470, #1691 ),
 .UNSPECIFIED., .F., .F.,
 ( 4, 2, 4 ),
 ( 4.462636793144160676E-07, 0.001879885123570646096, 0.003759323983461977832 ),
 .UNSPECIFIED. ) ;
#12962 = LINE ( 'NONE', #13106, #6564 ) ;
#12963 = CYLINDRICAL_SURFACE ( 'NONE', #14350, 8.400000000000000355 ) ;
#12964 = DIRECTION ( 'NONE',  ( -0.9031264002077605824, -0.4293747841312666180, -1.438198019250786829E-18 ) ) ;
#12965 = DIRECTION ( 'NONE',  ( 1.000000000000000000, 0.000000000000000000, 0.000000000000000000 ) ) ;
#12966 = EDGE_LOOP ( 'NONE', ( #11526, #14986 ) ) ;
#12967 = CARTESIAN_POINT ( 'NONE',  ( -14.40394475573011945, -4.794738323547945491, 16.99999999999999645 ) ) ;
#12968 = DIRECTION ( 'NONE',  ( 0.000000000000000000, 0.000000000000000000, 1.000000000000000000 ) ) ;
#12969 = EDGE_LOOP ( 'NONE', ( #12551, #4688, #2877, #1669, #8805 ) ) ;
#12970 = DIRECTION ( 'NONE',  ( 0.9995917534020515305, -0.02857142857142857054, 0.000000000000000000 ) ) ;
#12971 = FACE_OUTER_BOUND ( 'NONE', #12533, .T. ) ;
#12972 = CIRCLE ( 'NONE', #9308, 3.799999999999999378 ) ;
#12973 = B_SPLINE_CURVE_WITH_KNOTS ( 'NONE', 3,
 ( #11739, #199, #6056, #11656, #114, #11958, #5914, #9513 ),
 .UNSPECIFIED., .F., .F.,
 ( 4, 2, 2, 4 ),
 ( 1.984117563342565173E-07, 0.001895214258086353387, 0.002842722181251365696, 0.003790230104416377789 ),
 .UNSPECIFIED. ) ;
#12974 = CARTESIAN_POINT ( 'NONE',  ( 1.599999999999999867, -5.408326913195983465, -0.8000000000000000444 ) ) ;
#12975 = ORIENTED_EDGE ( 'NONE', *, *, #3261, .T. ) ;
#12976 = SURFACE_STYLE_FILL_AREA ( #1076 ) ;
#12977 = ORIENTED_EDGE ( 'NONE', *, *, #11950, .T. ) ;
#12978 = EDGE_LOOP ( 'NONE', ( #7277, #7581, #10637, #2560 ) ) ;
#12979 = ORIENTED_EDGE ( 'NONE', *, *, #3209, .F. ) ;
#12980 = DIRECTION ( 'NONE',  ( 0.000000000000000000, 0.000000000000000000, 1.000000000000000000 ) ) ;
#12981 = CARTESIAN_POINT ( 'NONE',  ( 19.20634328910001543, -26.21503864878155099, -2.000000000000000000 ) ) ;
#12982 = CARTESIAN_POINT ( 'NONE',  ( 2.789999999999999147, 1.621424371464993087E-13, -15.47981323787947794 ) ) ;
#12983 = CARTESIAN_POINT ( 'NONE',  ( 4.098876516494237640E-16, -15.96500990068138570, 18.34424029220106078 ) ) ;
#12984 = AXIS2_PLACEMENT_3D ( 'NONE', #14919, #3080, #9222 ) ;
#12985 = CARTESIAN_POINT ( 'NONE',  ( 0.4522159373304753816, -3.429166897524540403, 16.32199768300078802 ) ) ;
#12986 = VERTEX_POINT ( 'NONE', #9851 ) ;
#12987 = CYLINDRICAL_SURFACE ( 'NONE', #5581, 13.19999999999999929 ) ;
#12988 = VECTOR ( 'NONE', #6212, 1000.000000000000000 ) ;
#12989 = ORIENTED_EDGE ( 'NONE', *, *, #4440, .T. ) ;
#12990 = DIRECTION ( 'NONE',  ( 1.000000000000000000, 0.000000000000000000, 0.000000000000000000 ) ) ;
#12991 = CARTESIAN_POINT ( 'NONE',  ( 1.039999999999998259, -12.83329210556822986, -12.55714665600000757 ) ) ;
#12992 = ORIENTED_EDGE ( 'NONE', *, *, #2424, .T. ) ;
#12993 = ORIENTED_EDGE ( 'NONE', *, *, #2898, .F. ) ;
#12994 = EDGE_CURVE ( 'NONE', #10552, #3410, #5789, .T. ) ;
#12995 = DIRECTION ( 'NONE',  ( -1.000000000000000000, -0.000000000000000000, -0.000000000000000000 ) ) ;
#12996 = ORIENTED_EDGE ( 'NONE', *, *, #364, .F. ) ;
#12997 = CARTESIAN_POINT ( 'NONE',  ( 2.789999999999999147, -7.909232158574647009, -24.34211360614308006 ) ) ;
#12998 = ADVANCED_FACE ( 'NONE', ( #14626 ), #7402, .T. ) ;
#12999 = CARTESIAN_POINT ( 'NONE',  ( -14.40394475573011768, -16.79473832354794993, 22.00000000000000000 ) ) ;
#13000 = CARTESIAN_POINT ( 'NONE',  ( 1.749999999999999778, -12.55714665599996138, 12.83329210556827249 ) ) ;
#13001 = DIRECTION ( 'NONE',  ( 0.000000000000000000, 0.000000000000000000, 1.000000000000000000 ) ) ;
#13002 = ORIENTED_EDGE ( 'NONE', *, *, #2621, .F. ) ;
#13003 = DIRECTION ( 'NONE',  ( -1.000000000000000000, -0.000000000000000000, -0.000000000000000000 ) ) ;
#13004 = DIRECTION ( 'NONE',  ( 0.000000000000000000, 0.000000000000000000, 1.000000000000000000 ) ) ;
#13005 = ORIENTED_EDGE ( 'NONE', *, *, #14242, .T. ) ;
#13006 = EDGE_CURVE ( 'NONE', #14624, #7854, #12065, .T. ) ;
#13007 = ADVANCED_FACE ( 'NONE', ( #14777 ), #6465, .T. ) ;
#13008 = ORIENTED_EDGE ( 'NONE', *, *, #9748, .F. ) ;
#13009 = ORIENTED_EDGE ( 'NONE', *, *, #7945, .T. ) ;
#13010 = FACE_BOUND ( 'NONE', #14040, .T. ) ;
#13011 = CARTESIAN_POINT ( 'NONE',  ( 2.789999999999999147, 7.909232158575156824, -24.34211360614291664 ) ) ;
#13012 = CARTESIAN_POINT ( 'NONE',  ( 0.000000000000000000, 18.28042085475278000, 15.74360496233386719 ) ) ;
#13013 = APPLICATION_CONTEXT ( 'automotive_design' ) ;
#13014 = DIRECTION ( 'NONE',  ( -0.000000000000000000, -0.000000000000000000, -1.000000000000000000 ) ) ;
#13015 = CARTESIAN_POINT ( 'NONE',  ( 0.0001048300153468720319, 20.67846228565678146, -12.51925356660738053 ) ) ;
#13016 = PRODUCT_DEFINITION_SHAPE ( 'NONE', 'NONE',  #15228 ) ;
#13017 = CARTESIAN_POINT ( 'NONE',  ( 0.000000000000000000, -22.25075486061745167, 9.324097380959385006 ) ) ;
#13018 = ORIENTED_EDGE ( 'NONE', *, *, #9700, .F. ) ;
#13019 = CARTESIAN_POINT ( 'NONE',  ( 2.765633920072242180, 22.71065055754465689, -9.836394144775473691 ) ) ;
#13020 = DIRECTION ( 'NONE',  ( 1.000000000000000000, 0.000000000000000000, 0.000000000000000000 ) ) ;
#13021 = CYLINDRICAL_SURFACE ( 'NONE', #1945, 3.799999999999998934 ) ;
#13022 = CARTESIAN_POINT ( 'NONE',  ( 0.000000000000000000, -20.62201879784905501, -12.52067188844372936 ) ) ;
#13023 = EDGE_CURVE ( 'NONE', #14244, #8517, #5800, .T. ) ;
#13024 = ORIENTED_EDGE ( 'NONE', *, *, #2884, .F. ) ;
#13025 = ORIENTED_EDGE ( 'NONE', *, *, #14767, .F. ) ;
#13026 = EDGE_CURVE ( 'NONE', #3477, #1632, #7817, .T. ) ;
#13027 = EDGE_CURVE ( 'NONE', #8127, #5482, #2851, .T. ) ;
#13028 = VERTEX_POINT ( 'NONE', #8846 ) ;
#13029 = LINE ( 'NONE', #11875, #3386 ) ;
#13030 = DIRECTION ( 'NONE',  ( 0.000000000000000000, 0.000000000000000000, 1.000000000000000000 ) ) ;
#13031 = CARTESIAN_POINT ( 'NONE',  ( 1.749999999999999778, -12.83329210556841282, 12.55714665599981927 ) ) ;
#13032 = CARTESIAN_POINT ( 'NONE',  ( 0.1855657389739088781, -25.39738473785004302, 5.253342437939627629 ) ) ;
#13033 = DIRECTION ( 'NONE',  ( 1.632700458502094890E-19, 3.006102310110810585E-18, -1.000000000000000000 ) ) ;
#13034 = LINE ( 'NONE', #6836, #8647 ) ;
#13035 = EDGE_CURVE ( 'NONE', #15218, #9857, #13539, .T. ) ;
#13036 = ORIENTED_EDGE ( 'NONE', *, *, #14557, .T. ) ;
#13037 = CARTESIAN_POINT ( 'NONE',  ( 1.039999999999995817, -27.76164181293048472, -4.147968289691575272 ) ) ;
#13038 = DIRECTION ( 'NONE',  ( 0.000000000000000000, 0.000000000000000000, 1.000000000000000000 ) ) ;
#13039 = VERTEX_POINT ( 'NONE', #14549 ) ;
#13040 = CARTESIAN_POINT ( 'NONE',  ( 2.789999999999999147, 20.62201879784912606, 12.52067188844359080 ) ) ;
#13041 = AXIS2_PLACEMENT_3D ( 'NONE', #12649, #2133, #976 ) ;
#13042 = DIRECTION ( 'NONE',  ( 1.000000000000000000, 0.000000000000000000, 0.000000000000000000 ) ) ;
#13043 = ORIENTED_EDGE ( 'NONE', *, *, #4118, .T. ) ;
#13044 = ORIENTED_EDGE ( 'NONE', *, *, #646, .F. ) ;
#13045 = VERTEX_POINT ( 'NONE', #1710 ) ;
#13046 = ORIENTED_EDGE ( 'NONE', *, *, #11482, .T. ) ;
#13047 = CARTESIAN_POINT ( 'NONE',  ( 1.039999999999996039, 27.68468304288258963, 4.633866840649018215 ) ) ;
#13048 = CARTESIAN_POINT ( 'NONE',  ( 2.783025342027734439, -23.92335783895641299, 5.408388659523998498 ) ) ;
#13049 = AXIS2_PLACEMENT_3D ( 'NONE', #10949, #12026, #2668 ) ;
#13050 = CARTESIAN_POINT ( 'NONE',  ( 0.1920563539683084187, 15.58455734132166981, 2.883512197589065185 ) ) ;
#13051 = CARTESIAN_POINT ( 'NONE',  ( 2.236220312281013811, -11.41743294611066339, -12.52687487503431463 ) ) ;
#13052 = EDGE_CURVE ( 'NONE', #761, #14623, #1619, .T. ) ;
#13053 = CARTESIAN_POINT ( 'NONE',  ( 2.789999999999999147, -12.52067188844365830, 20.62201879784908698 ) ) ;
#13054 = ORIENTED_EDGE ( 'NONE', *, *, #6466, .F. ) ;
#13055 = LINE ( 'NONE', #5018, #5820 ) ;
#13056 = CIRCLE ( 'NONE', #9878, 4.000000000000000000 ) ;
#13057 = ORIENTED_EDGE ( 'NONE', *, *, #2679, .F. ) ;
#13058 = CARTESIAN_POINT ( 'NONE',  ( 2.789999999999999147, 14.18181402625769749, -19.91106274590499225 ) ) ;
#13059 = FACE_OUTER_BOUND ( 'NONE', #1087, .T. ) ;
#13060 = EDGE_CURVE ( 'NONE', #6955, #5808, #8540, .T. ) ;
#13061 = EDGE_LOOP ( 'NONE', ( #6660, #14705, #8439, #2635, #5395, #9230 ) ) ;
#13062 = ORIENTED_EDGE ( 'NONE', *, *, #10673, .F. ) ;
#13063 = CARTESIAN_POINT ( 'NONE',  ( 2.790000000000076419, -22.38018801136469094, -9.515416771311432598 ) ) ;
#13064 = ORIENTED_EDGE ( 'NONE', *, *, #8427, .F. ) ;
#13065 = CARTESIAN_POINT ( 'NONE',  ( 0.000000000000000000, 3.361026734705063745E-15, 7.799999999999990052 ) ) ;
#13066 = CARTESIAN_POINT ( 'NONE',  ( -14.40394475573011768, -7.794738323547949932, 16.99999999999999645 ) ) ;
#13067 = SHAPE_REPRESENTATION ( 'spacer', ( #1376 ), #2126 ) ;
#13068 = EDGE_CURVE ( 'NONE', #7278, #4522, #7472, .T. ) ;
#13069 = DIRECTION ( 'NONE',  ( -1.000000000000000000, 0.000000000000000000, -0.000000000000000000 ) ) ;
#13070 = CARTESIAN_POINT ( 'NONE',  ( 93.34550147531103903, 3.654933296868752457, -2.000000000000000888 ) ) ;
#13071 = ORIENTED_EDGE ( 'NONE', *, *, #7585, .T. ) ;
#13072 = DIRECTION ( 'NONE',  ( -1.000000000000000000, -0.000000000000000000, 0.000000000000000000 ) ) ;
#13073 = EDGE_CURVE ( 'NONE', #14059, #13883, #7746, .T. ) ;
#13074 = DIRECTION ( 'NONE',  ( -1.000000000000000000, -0.000000000000000000, -0.000000000000000000 ) ) ;
#13075 = ORIENTED_EDGE ( 'NONE', *, *, #4574, .T. ) ;
#13076 = CARTESIAN_POINT ( 'NONE',  ( 2.781248467066446572, 13.40591150985955871, -5.214906618939568972 ) ) ;
#13077 = VERTEX_POINT ( 'NONE', #10082 ) ;
#13078 = ORIENTED_EDGE ( 'NONE', *, *, #12852, .T. ) ;
#13079 = CARTESIAN_POINT ( 'NONE',  ( 86.17559721729969624, 12.01344854909570259, 2.999999999999999112 ) ) ;
#13080 = CARTESIAN_POINT ( 'NONE',  ( 2.789999999999999147, -15.04425356660744839, -18.18163861606288378 ) ) ;
#13081 = AXIS2_PLACEMENT_3D ( 'NONE', #14358, #3592, #3820 ) ;
#13082 = DIRECTION ( 'NONE',  ( -1.000000000000000000, -0.000000000000000000, -0.000000000000000000 ) ) ;
#13083 = B_SPLINE_CURVE_WITH_KNOTS ( 'NONE', 3,
 ( #5507, #4348, #13726, #9035 ),
 .UNSPECIFIED., .F., .F.,
 ( 4, 4 ),
 ( 1.988537749986029444E-07, 0.0002742066915202718549 ),
 .UNSPECIFIED. ) ;
#13084 = DIRECTION ( 'NONE',  ( -0.000000000000000000, -0.000000000000000000, 1.000000000000000000 ) ) ;
#13085 = DIRECTION ( 'NONE',  ( 0.4570747303910190351, -0.8894282943767740646, 6.847307257068341160E-17 ) ) ;
#13086 = CIRCLE ( 'NONE', #10655, 4.999999999999997335 ) ;
#13087 = DIRECTION ( 'NONE',  ( -1.000000000000000000, -0.000000000000000000, -0.000000000000000000 ) ) ;
#13088 = CIRCLE ( 'NONE', #6735, 4.000000000000000000 ) ;
#13089 = VERTEX_POINT ( 'NONE', #468 ) ;
#13090 = PLANE ( 'NONE',  #6596 ) ;
#13091 = VECTOR ( 'NONE', #14015, 1000.000000000000000 ) ;
#13092 = PLANE ( 'NONE',  #1030 ) ;
#13093 = DIRECTION ( 'NONE',  ( 1.000000000000000000, 0.000000000000000000, 0.000000000000000000 ) ) ;
#13094 = B_SPLINE_CURVE_WITH_KNOTS ( 'NONE', 3,
 ( #4794, #9545, #13233, #2711, #11687, #11835 ),
 .UNSPECIFIED., .F., .F.,
 ( 4, 2, 4 ),
 ( 2.032124546189621919E-07, 0.001878594002992306630, 0.003756984793529993989 ),
 .UNSPECIFIED. ) ;
#13095 = CYLINDRICAL_SURFACE ( 'NONE', #12907, 2.524999999999995914 ) ;
#13096 = ORIENTED_EDGE ( 'NONE', *, *, #15017, .F. ) ;
#13097 = ORIENTED_EDGE ( 'NONE', *, *, #4189, .T. ) ;
#13098 = AXIS2_PLACEMENT_3D ( 'NONE', #2068, #11587, #6835 ) ;
#13099 = AXIS2_PLACEMENT_3D ( 'NONE', #3881, #5836, #3585 ) ;
#13100 = ADVANCED_FACE ( 'NONE', ( #5186 ), #8681, .F. ) ;
#13101 = ORIENTED_EDGE ( 'NONE', *, *, #14249, .T. ) ;
#13102 = AXIS2_PLACEMENT_3D ( 'NONE', #3753, #11817, #3681 ) ;
#13103 = APPLICATION_CONTEXT ( 'automotive_design' ) ;
#13104 = DIRECTION ( 'NONE',  ( -1.000000000000000000, -0.000000000000000000, -0.000000000000000000 ) ) ;
#13105 = CARTESIAN_POINT ( 'NONE',  ( 61.98919079003883326, 3.953582723775848962, 2.999999999999999112 ) ) ;
#13106 = CARTESIAN_POINT ( 'NONE',  ( -15.94493884710238696, -7.321218896460230496, -3.800000000000000266 ) ) ;
#13107 = DIRECTION ( 'NONE',  ( 0.000000000000000000, 0.000000000000000000, -1.000000000000000000 ) ) ;
#13108 = DIRECTION ( 'NONE',  ( 0.000000000000000000, 0.000000000000000000, -1.000000000000000000 ) ) ;
#13109 = DIRECTION ( 'NONE',  ( 0.000000000000000000, 0.000000000000000000, 1.000000000000000000 ) ) ;
#13110 = EDGE_LOOP ( 'NONE', ( #10664, #3684, #8717, #5087 ) ) ;
#13111 = CARTESIAN_POINT ( 'NONE',  ( 2.789999999999999147, -20.62201879784904079, -12.52067188844374179 ) ) ;
#13112 = CARTESIAN_POINT ( 'NONE',  ( 0.07181523211952839381, -10.24584646439522828, -23.19431517146944088 ) ) ;
#13113 = VECTOR ( 'NONE', #1341, 1000.000000000000000 ) ;
#13114 = EDGE_CURVE ( 'NONE', #1743, #9942, #3090, .T. ) ;
#13115 = VECTOR ( 'NONE', #13470, 1000.000000000000000 ) ;
#13116 = EDGE_CURVE ( 'NONE', #14810, #11407, #9093, .T. ) ;
#13117 = ORIENTED_EDGE ( 'NONE', *, *, #10811, .T. ) ;
#13118 = CARTESIAN_POINT ( 'NONE',  ( 0.1882238782932344479, 19.18368891937516452, -17.47009390565470000 ) ) ;
#13119 = CARTESIAN_POINT ( 'NONE',  ( 1.039999999999996927, 12.55714665600005375, -12.83329210556818545 ) ) ;
#13120 = CIRCLE ( 'NONE', #13874, 2.524999999999996358 ) ;
#13121 = SURFACE_SIDE_STYLE ('',( #8433 ) ) ;
#13122 = ORIENTED_EDGE ( 'NONE', *, *, #2967, .F. ) ;
#13123 = B_SPLINE_CURVE_WITH_KNOTS ( 'NONE', 3,
 ( #14697, #13294, #4166, #2774 ),
 .UNSPECIFIED., .F., .F.,
 ( 4, 4 ),
 ( 2.451234579287565992E-07, 0.0006917187676826499999 ),
 .UNSPECIFIED. ) ;
#13124 =( LENGTH_UNIT ( ) NAMED_UNIT ( * ) SI_UNIT ( .MILLI., .METRE. ) );
#13125 = ORIENTED_EDGE ( 'NONE', *, *, #9224, .T. ) ;
#13126 = EDGE_LOOP ( 'NONE', ( #13618, #6916, #14192, #10791 ) ) ;
#13127 = ORIENTED_EDGE ( 'NONE', *, *, #14313, .T. ) ;
#13128 = CARTESIAN_POINT ( 'NONE',  ( 18.87754531448929995, -24.24225080111726527, 5.000000000000000000 ) ) ;
#13129 = AXIS2_PLACEMENT_3D ( 'NONE', #1965, #4494, #1027 ) ;
#13130 = CARTESIAN_POINT ( 'NONE',  ( 2.031033491000347357, 12.05173163741723030, 24.80232951178382805 ) ) ;
#13131 = VECTOR ( 'NONE', #12779, 1000.000000000000114 ) ;
#13132 = CARTESIAN_POINT ( 'NONE',  ( 2.789999999999999147, 5.249430348645936384, -12.98979500319688718 ) ) ;
#13133 = CARTESIAN_POINT ( 'NONE',  ( 80.00000000000000000, 0.000000000000000000, 7.000000000000000000 ) ) ;
#13134 = EDGE_CURVE ( 'NONE', #5814, #14639, #1379, .T. ) ;
#13135 = ADVANCED_BREP_SHAPE_REPRESENTATION ( '', ( #3266, #1376 ), #4341 ) ;
#13136 = CARTESIAN_POINT ( 'NONE',  ( 14.40394475573011945, -10.79473832354794460, 3.000000000000000000 ) ) ;
#13137 = EDGE_CURVE ( 'NONE', #1510, #2255, #3371, .T. ) ;
#13138 = CARTESIAN_POINT ( 'NONE',  ( -10.00000000000000000, 0.000000000000000000, 0.000000000000000000 ) ) ;
#13139 = EDGE_CURVE ( 'NONE', #3376, #7725, #15154, .T. ) ;
#13140 = ORIENTED_EDGE ( 'NONE', *, *, #5894, .T. ) ;
#13141 = CARTESIAN_POINT ( 'NONE',  ( -14.40394475573011945, -10.79473832354794283, -3.799999999999999822 ) ) ;
#13142 = AXIS2_PLACEMENT_3D ( 'NONE', #7406, #6241, #10923 ) ;
#13143 = ADVANCED_FACE ( 'NONE', ( #2083 ), #7928, .T. ) ;
#13144 = ORIENTED_EDGE ( 'NONE', *, *, #6839, .F. ) ;
#13145 = PLANE ( 'NONE',  #11174 ) ;
#13146 = PRODUCT_DEFINITION_SHAPE ( 'NONE', 'NONE',  #15232 ) ;
#13147 = CARTESIAN_POINT ( 'NONE',  ( -14.40394475573011945, -4.794738323547945491, 22.00000000000000000 ) ) ;
#13148 = AXIS2_PLACEMENT_3D ( 'NONE', #6459, #11134, #1545 ) ;
#13149 = ORIENTED_EDGE ( 'NONE', *, *, #10056, .T. ) ;
#13150 = ORIENTED_EDGE ( 'NONE', *, *, #13987, .T. ) ;
#13151 = AXIS2_PLACEMENT_3D ( 'NONE', #10062, #12654, #11506 ) ;
#13152 = B_SPLINE_CURVE_WITH_KNOTS ( 'NONE', 3,
 ( #9672, #10979, #7609, #444, #3991, #14372, #7533, #5232 ),
 .UNSPECIFIED., .F., .F.,
 ( 4, 2, 2, 4 ),
 ( 4.663089536348421000E-07, 0.001898630414085407565, 0.002847712466651294936, 0.003796794519217182307 ),
 .UNSPECIFIED. ) ;
#13153 = CARTESIAN_POINT ( 'NONE',  ( -5.209999999999999964, 0.000000000000000000, 0.000000000000000000 ) ) ;
#13154 = EDGE_LOOP ( 'NONE', ( #347, #9333, #8377, #5926 ) ) ;
#13155 = CARTESIAN_POINT ( 'NONE',  ( 1.749999999999998002, 0.000000000000000000, 0.000000000000000000 ) ) ;
#13156 = LINE ( 'NONE', #162, #4409 ) ;
#13157 = DIRECTION ( 'NONE',  ( 1.000000000000000000, 0.000000000000000000, 0.000000000000000000 ) ) ;
#13158 = AXIS2_PLACEMENT_3D ( 'NONE', #9539, #11908, #65 ) ;
#13159 = DIRECTION ( 'NONE',  ( 0.000000000000000000, 0.000000000000000000, -1.000000000000000000 ) ) ;
#13160 = ORIENTED_EDGE ( 'NONE', *, *, #6307, .T. ) ;
#13161 = CIRCLE ( 'NONE', #6549, 2.999999999999988898 ) ;
#13162 = DIRECTION ( 'NONE',  ( -0.000000000000000000, -0.000000000000000000, 1.000000000000000000 ) ) ;
#13163 = CARTESIAN_POINT ( 'NONE',  ( 2.783025306068355853, -18.43727551351019045, -16.17543236988008815 ) ) ;
#13164 = AXIS2_PLACEMENT_3D ( 'NONE', #15074, #1943, #931 ) ;
#13165 = AXIS2_PLACEMENT_3D ( 'NONE', #1794, #4105, #8785 ) ;
#13166 = EDGE_CURVE ( 'NONE', #9661, #9629, #11455, .T. ) ;
#13167 = ORIENTED_EDGE ( 'NONE', *, *, #5136, .F. ) ;
#13168 = CARTESIAN_POINT ( 'NONE',  ( 0.7795480763126745316, 12.70439593876660567, 11.98750039041498461 ) ) ;
#13169 = ORIENTED_EDGE ( 'NONE', *, *, #1571, .T. ) ;
#13170 = ORIENTED_EDGE ( 'NONE', *, *, #1758, .F. ) ;
#13171 = CARTESIAN_POINT ( 'NONE',  ( 8.961831343790189308, 9.104486995144791095, -131.1575142076926852 ) ) ;
#13172 = FACE_BOUND ( 'NONE', #7435, .T. ) ;
#13173 = AXIS2_PLACEMENT_3D ( 'NONE', #6520, #14755, #13208 ) ;
#13174 = PLANE ( 'NONE',  #7247 ) ;
#13175 = FACE_OUTER_BOUND ( 'NONE', #14724, .T. ) ;
#13176 = EDGE_CURVE ( 'NONE', #5857, #2934, #7075, .T. ) ;
#13177 = VECTOR ( 'NONE', #5839, 1000.000000000000000 ) ;
#13178 = FACE_OUTER_BOUND ( 'NONE', #12407, .T. ) ;
#13179 = VECTOR ( 'NONE', #272, 1000.000000000000114 ) ;
#13180 = ORIENTED_EDGE ( 'NONE', *, *, #13431, .F. ) ;
#13181 = FACE_OUTER_BOUND ( 'NONE', #6149, .T. ) ;
#13182 = CYLINDRICAL_SURFACE ( 'NONE', #11827, 4.000000000000000000 ) ;
#13183 = VECTOR ( 'NONE', #8370, 1000.000000000000114 ) ;
#13184 = CARTESIAN_POINT ( 'NONE',  ( 67.23404255319145761, 28.93147646537026318, 6.000000000000000000 ) ) ;
#13185 = CARTESIAN_POINT ( 'NONE',  ( -7.625032001148274383E-14, 9.515416771311183908, 22.38018801136479397 ) ) ;
#13186 = ORIENTED_EDGE ( 'NONE', *, *, #7955, .T. ) ;
#13187 = EDGE_LOOP ( 'NONE', ( #342, #8103, #1077, #12562, #14527, #6401 ) ) ;
#13188 = ORIENTED_EDGE ( 'NONE', *, *, #9923, .F. ) ;
#13189 = VECTOR ( 'NONE', #4737, 1000.000000000000000 ) ;
#13190 = PRESENTATION_LAYER_ASSIGNMENT (  '', '', ( #14925 ) ) ;
#13191 = DIRECTION ( 'NONE',  ( -1.000000000000000000, -0.000000000000000000, -0.000000000000000000 ) ) ;
#13192 = DIRECTION ( 'NONE',  ( -1.000000000000000000, -0.000000000000000000, -0.000000000000000000 ) ) ;
#13193 = CIRCLE ( 'NONE', #1662, 14.01039946648074341 ) ;
#13194 = CIRCLE ( 'NONE', #14687, 6.000000000000000888 ) ;
#13195 = DIRECTION ( 'NONE',  ( 0.000000000000000000, 0.000000000000000000, 1.000000000000000000 ) ) ;
#13196 = CARTESIAN_POINT ( 'NONE',  ( 2.789999999999999147, -19.91106274590524094, 14.18181402625735466 ) ) ;
#13197 = CARTESIAN_POINT ( 'NONE',  ( 2.008221563957562463E-18, 3.697505841436304973E-17, -7.799999999999999822 ) ) ;
#13198 = DIRECTION ( 'NONE',  ( -1.000000000000000000, -0.000000000000000000, 0.000000000000000000 ) ) ;
#13199 = EDGE_CURVE ( 'NONE', #12618, #7983, #12191, .T. ) ;
#13200 = VERTEX_POINT ( 'NONE', #10313 ) ;
#13201 = DIRECTION ( 'NONE',  ( 1.000000000000000000, 0.000000000000000000, -1.576560579138137530E-17 ) ) ;
#13202 = CARTESIAN_POINT ( 'NONE',  ( 2.765633920072238627, 12.59161484032942901, -21.30679549418617924 ) ) ;
#13203 = ORIENTED_EDGE ( 'NONE', *, *, #321, .F. ) ;
#13204 = CARTESIAN_POINT ( 'NONE',  ( 15.21482963846748504, 16.90833299098317610, 7.000000000000006217 ) ) ;
#13205 = DIRECTION ( 'NONE',  ( 0.000000000000000000, 0.000000000000000000, -1.000000000000000000 ) ) ;
#13206 = EDGE_CURVE ( 'NONE', #13461, #13319, #2628, .T. ) ;
#13207 = CIRCLE ( 'NONE', #15188, 5.899999999999999467 ) ;
#13208 = DIRECTION ( 'NONE',  ( 0.000000000000000000, 0.000000000000000000, 1.000000000000000000 ) ) ;
#13209 = ORIENTED_EDGE ( 'NONE', *, *, #12731, .F. ) ;
#13210 = CIRCLE ( 'NONE', #3166, 2.524999999999995914 ) ;
#13211 = CIRCLE ( 'NONE', #10523, 2.524999999999995914 ) ;
#13212 = CARTESIAN_POINT ( 'NONE',  ( 0.02531912748464674665, -11.36963888406694068, 9.232963481057725019 ) ) ;
#13213 = CARTESIAN_POINT ( 'NONE',  ( 88.84370878116858705, 10.64188714589527507, 4.000000000000000000 ) ) ;
#13214 = VERTEX_POINT ( 'NONE', #9085 ) ;
#13215 = EDGE_LOOP ( 'NONE', ( #2035, #8564, #14459, #8935, #9207, #5329 ) ) ;
#13216 = ORIENTED_EDGE ( 'NONE', *, *, #12281, .F. ) ;
#13217 = LINE ( 'NONE', #449, #14410 ) ;
#13218 = PRODUCT_RELATED_PRODUCT_CATEGORY ( 'part', '', ( #13509 ) ) ;
#13219 = DIRECTION ( 'NONE',  ( -0.000000000000000000, 0.000000000000000000, -1.000000000000000000 ) ) ;
#13220 = EDGE_CURVE ( 'NONE', #7890, #2234, #9496, .T. ) ;
#13221 = EDGE_CURVE ( 'NONE', #1932, #1234, #4106, .T. ) ;
#13222 = CARTESIAN_POINT ( 'NONE',  ( 1.749999999999999778, 17.29145405592688789, 4.835383649608534284 ) ) ;
#13223 = CARTESIAN_POINT ( 'NONE',  ( 1.885839528871394943, -12.27244837507604025, -12.77651625388912038 ) ) ;
#13224 = DIRECTION ( 'NONE',  ( -1.000000000000000000, -0.000000000000000000, -0.000000000000000000 ) ) ;
#13225 = CARTESIAN_POINT ( 'NONE',  ( 2.718131914667133220, 23.19485392143227642, -10.24630254990492340 ) ) ;
#13226 = VECTOR ( 'NONE', #3964, 1000.000000000000000 ) ;
#13227 = ORIENTED_EDGE ( 'NONE', *, *, #7879, .F. ) ;
#13228 = DIRECTION ( 'NONE',  ( -1.000000000000000000, -0.000000000000000000, -0.000000000000000000 ) ) ;
#13229 = EDGE_CURVE ( 'NONE', #6338, #10607, #5100, .T. ) ;
#13230 = ORIENTED_EDGE ( 'NONE', *, *, #7486, .T. ) ;
#13231 = ORIENTED_EDGE ( 'NONE', *, *, #11861, .F. ) ;
#13232 = CIRCLE ( 'NONE', #2191, 5.999999999999999112 ) ;
#13233 = CARTESIAN_POINT ( 'NONE',  ( 2.604434283110813819, -22.53097606932974983, -12.84444904262050002 ) ) ;
#13234 = CARTESIAN_POINT ( 'NONE',  ( 0.2076373605413182333, -14.94126095370957863, -5.278564329441158165 ) ) ;
#13235 = ADVANCED_FACE ( 'NONE', ( #3395 ), #5484, .F. ) ;
#13236 = ORIENTED_EDGE ( 'NONE', *, *, #14631, .T. ) ;
#13237 = FACE_OUTER_BOUND ( 'NONE', #2297, .T. ) ;
#13238 = EDGE_CURVE ( 'NONE', #12774, #3044, #11602, .T. ) ;
#13239 = VERTEX_POINT ( 'NONE', #9316 ) ;
#13240 = CYLINDRICAL_SURFACE ( 'NONE', #5989, 2.524999999999999023 ) ;
#13241 = DIRECTION ( 'NONE',  ( -0.8893705212896292345, 0.4571871344001417481, 0.000000000000000000 ) ) ;
#13242 = VECTOR ( 'NONE', #3247, 1000.000000000000000 ) ;
#13243 = CARTESIAN_POINT ( 'NONE',  ( 2.789999999999999147, 15.04425356660790136, -20.70663861606255196 ) ) ;
#13244 = VERTEX_POINT ( 'NONE', #6150 ) ;
#13245 = CARTESIAN_POINT ( 'NONE',  ( 0.000000000000000000, 1.621424371464993087E-13, -15.47981323787947794 ) ) ;
#13246 = CARTESIAN_POINT ( 'NONE',  ( 0.000000000000000000, -25.59481291497571220, -1.787276233276378314E-13 ) ) ;
#13247 = ORIENTED_EDGE ( 'NONE', *, *, #11327, .T. ) ;
#13248 = CARTESIAN_POINT ( 'NONE',  ( 1.006169830977205581, -4.228366069762346413, 4.000000000000000000 ) ) ;
#13249 = DIRECTION ( 'NONE',  ( 0.000000000000000000, 0.000000000000000000, 1.000000000000000000 ) ) ;
#13250 = ORIENTED_EDGE ( 'NONE', *, *, #14274, .T. ) ;
#13251 = VERTEX_POINT ( 'NONE', #9448 ) ;
#13252 = DIRECTION ( 'NONE',  ( -0.000000000000000000, -0.000000000000000000, 1.000000000000000000 ) ) ;
#13253 = AXIS2_PLACEMENT_3D ( 'NONE', #6670, #7826, #5603 ) ;
#13254 = DIRECTION ( 'NONE',  ( 0.000000000000000000, 0.000000000000000000, 1.000000000000000000 ) ) ;
#13255 = CARTESIAN_POINT ( 'NONE',  ( 56.98919079003883326, 3.953582723775848962, 2.999999999999999112 ) ) ;
#13256 = FACE_BOUND ( 'NONE', #1075, .T. ) ;
#13257 = CARTESIAN_POINT ( 'NONE',  ( 2.783068930044319433, 18.43696893154781691, -16.17493693894858353 ) ) ;
#13258 = ORIENTED_EDGE ( 'NONE', *, *, #9364, .F. ) ;
#13259 = CARTESIAN_POINT ( 'NONE',  ( 91.46153288930040048, 16.46030115554384565, 6.000000000000000000 ) ) ;
#13260 = LINE ( 'NONE', #5287, #2260 ) ;
#13261 = CARTESIAN_POINT ( 'NONE',  ( 1.885839517048285119, -4.239993951493086222, -17.20101185194004856 ) ) ;
#13262 = DIRECTION ( 'NONE',  ( -1.000000000000000000, -0.000000000000000000, -0.000000000000000000 ) ) ;
#13263 = ORIENTED_EDGE ( 'NONE', *, *, #9582, .F. ) ;
#13264 = ORIENTED_EDGE ( 'NONE', *, *, #9165, .T. ) ;
#13265 = VERTEX_POINT ( 'NONE', #2614 ) ;
#13266 = DIRECTION ( 'NONE',  ( 1.000000000000000000, 0.000000000000000000, 0.000000000000000000 ) ) ;
#13267 = EDGE_CURVE ( 'NONE', #952, #4433, #11942, .T. ) ;
#13268 = CARTESIAN_POINT ( 'NONE',  ( 80.82762530298222714, -19.99999999999999645, 4.000000000000003553 ) ) ;
#13269 = LINE ( 'NONE', #8883, #11648 ) ;
#13270 = DIRECTION ( 'NONE',  ( 0.1473126338456100803, -0.9890899796830768809, 0.000000000000000000 ) ) ;
#13271 = CARTESIAN_POINT ( 'NONE',  ( 2.136152509568735258, 16.44008199387299740, 5.087730618022634488 ) ) ;
#13272 = ORIENTED_EDGE ( 'NONE', *, *, #790, .F. ) ;
#13273 = LINE ( 'NONE', #12038, #9568 ) ;
#13274 = CARTESIAN_POINT ( 'NONE',  ( -7.922038997698610785E-14, 18.34439787333529992, -15.96555658743743145 ) ) ;
#13275 = ORIENTED_EDGE ( 'NONE', *, *, #5919, .F. ) ;
#13276 = CARTESIAN_POINT ( 'NONE',  ( -0.1085714285714285687, -3.798448662927795372, -0.8000000000000000444 ) ) ;
#13277 = CARTESIAN_POINT ( 'NONE',  ( 2.789999999999999147, 1.621424371464993087E-13, -15.47981323787947794 ) ) ;
#13278 = DIRECTION ( 'NONE',  ( -1.000000000000000000, -0.000000000000000000, -0.000000000000000000 ) ) ;
#13279 = ADVANCED_FACE ( 'NONE', ( #5993 ), #2386, .T. ) ;
#13280 = VERTEX_POINT ( 'NONE', #13047 ) ;
#13281 = EDGE_CURVE ( 'NONE', #5202, #4588, #14142, .T. ) ;
#13282 = DIRECTION ( 'NONE',  ( 0.02857142857142857401, -0.9995917534020515305, 0.000000000000000000 ) ) ;
#13283 = CARTESIAN_POINT ( 'NONE',  ( 0.006974771092476448643, 22.53337530003417655, -9.686319561460717154 ) ) ;
#13284 = ORIENTED_EDGE ( 'NONE', *, *, #14622, .F. ) ;
#13285 = ORIENTED_EDGE ( 'NONE', *, *, #58, .T. ) ;
#13286 = ORIENTED_EDGE ( 'NONE', *, *, #1986, .F. ) ;
#13287 = CARTESIAN_POINT ( 'NONE',  ( -5.209999999999999964, 0.000000000000000000, 0.000000000000000000 ) ) ;
#13288 = ADVANCED_FACE ( 'NONE', ( #13997, #3529, #4936, #8218, #11675, #8299, #3463, #2536 ), #14225, .F. ) ;
#13289 = CARTESIAN_POINT ( 'NONE',  ( 0.000000000000000000, -13.40591150984231916, 7.739906618939660810 ) ) ;
#13290 = FACE_BOUND ( 'NONE', #13769, .T. ) ;
#13291 = CARTESIAN_POINT ( 'NONE',  ( -10.00000000000000000, 0.000000000000000000, 0.000000000000000000 ) ) ;
#13292 = CARTESIAN_POINT ( 'NONE',  ( 2.765633920072242180, 22.71065055754465689, -9.836394144775473691 ) ) ;
#13293 = ORIENTED_EDGE ( 'NONE', *, *, #5081, .T. ) ;
#13294 = CARTESIAN_POINT ( 'NONE',  ( 0.007327564474061405535, -11.23174270417335663, 9.044896821682165466 ) ) ;
#13295 = ADVANCED_FACE ( 'NONE', ( #1300, #10682 ), #1161, .T. ) ;
#13296 = SURFACE_STYLE_FILL_AREA ( #7623 ) ;
#13297 = CIRCLE ( 'NONE', #9132, 2.999999999999975131 ) ;
#13298 = ORIENTED_EDGE ( 'NONE', *, *, #9287, .F. ) ;
#13299 = ORIENTED_EDGE ( 'NONE', *, *, #6490, .F. ) ;
#13300 = CARTESIAN_POINT ( 'NONE',  ( 2.789999999999999147, -12.52067188844336165, -20.62201879784926462 ) ) ;
#13301 = CARTESIAN_POINT ( 'NONE',  ( 1.749999999999998002, 19.67366047555558950, -20.02152543075324687 ) ) ;
#13302 = VERTEX_POINT ( 'NONE', #5010 ) ;
#13303 = EDGE_CURVE ( 'NONE', #7479, #6398, #10174, .T. ) ;
#13304 = UNCERTAINTY_MEASURE_WITH_UNIT (LENGTH_MEASURE( 1.000000000000000082E-05 ), #8541, 'distance_accuracy_value', 'NONE');
#13305 = CYLINDRICAL_SURFACE ( 'NONE', #6771, 8.400000000000000355 ) ;
#13306 = EDGE_CURVE ( 'NONE', #159, #14739, #1028, .T. ) ;
#13307 = ORIENTED_EDGE ( 'NONE', *, *, #10519, .T. ) ;
#13308 = AXIS2_PLACEMENT_3D ( 'NONE', #3980, #10966, #2521 ) ;
#13309 = LINE ( 'NONE', #1789, #10431 ) ;
#13310 = CARTESIAN_POINT ( 'NONE',  ( 0.5279273381794633568, -3.461047254864449307, 26.82026385750176445 ) ) ;
#13311 = EDGE_CURVE ( 'NONE', #5009, #10601, #7300, .T. ) ;
#13312 = EDGE_CURVE ( 'NONE', #6955, #5688, #12442, .T. ) ;
#13313 = CARTESIAN_POINT ( 'NONE',  ( 14.27437366993929579, -27.03703358530833967, 4.000000000000000000 ) ) ;
#13314 = FACE_OUTER_BOUND ( 'NONE', #12252, .T. ) ;
#13315 = CARTESIAN_POINT ( 'NONE',  ( 5.366045694719498695E-16, 9.514945144209063344, -22.37986894186662923 ) ) ;
#13316 = ORIENTED_EDGE ( 'NONE', *, *, #13717, .F. ) ;
#13317 = DIRECTION ( 'NONE',  ( -1.000000000000000000, 0.000000000000000000, 0.000000000000000000 ) ) ;
#13318 = CARTESIAN_POINT ( 'NONE',  ( 2.789999999999999147, 7.772527002114431482, 23.17675759782044054 ) ) ;
#13319 = VERTEX_POINT ( 'NONE', #10763 ) ;
#13320 = ORIENTED_EDGE ( 'NONE', *, *, #5772, .F. ) ;
#13321 = DIRECTION ( 'NONE',  ( 0.000000000000000000, 0.000000000000000000, 1.000000000000000000 ) ) ;
#13322 = CARTESIAN_POINT ( 'NONE',  ( 1.249999999999997558, 0.000000000000000000, 0.000000000000000000 ) ) ;
#13323 = DIRECTION ( 'NONE',  ( 1.000000000000000000, 0.000000000000000000, 0.000000000000000000 ) ) ;
#13324 = ADVANCED_FACE ( 'NONE', ( #3610 ), #1236, .T. ) ;
#13325 = ADVANCED_FACE ( 'NONE', ( #4775 ), #8442, .T. ) ;
#13326 = CARTESIAN_POINT ( 'NONE',  ( 93.34550147531103903, 3.654933296868752457, 2.999999999999999112 ) ) ;
#13328 = ORIENTED_EDGE ( 'NONE', *, *, #4607, .F. ) ;
#13327 = EDGE_CURVE ( 'NONE', #10097, #546, #8760, .T. ) ;
#13329 = CARTESIAN_POINT ( 'NONE',  ( 0.000000000000000000, 2.680914349914567470E-13, -25.59481291497571220 ) ) ;
#13330 = FACE_OUTER_BOUND ( 'NONE', #13513, .T. ) ;
#13331 = CARTESIAN_POINT ( 'NONE',  ( 2.010451919658890585, -4.029281904976513395, -16.99607982911245330 ) ) ;
#13332 = DIRECTION ( 'NONE',  ( 0.000000000000000000, 0.000000000000000000, 1.000000000000000000 ) ) ;
#13333 = EDGE_LOOP ( 'NONE', ( #481, #10894, #2467, #7325 ) ) ;
#13334 = VERTEX_POINT ( 'NONE', #8526 ) ;
#13335 = ADVANCED_FACE ( 'NONE', ( #8749 ), #9902, .F. ) ;
#13336 = AXIS2_PLACEMENT_3D ( 'NONE', #11807, #4993, #7287 ) ;
#13337 = ORIENTED_EDGE ( 'NONE', *, *, #2538, .T. ) ;
#13338 = CARTESIAN_POINT ( 'NONE',  ( 4.000000000000000888, 4.898587196589413815E-16, -7.800000000000010481 ) ) ;
#13339 = DIRECTION ( 'NONE',  ( 0.000000000000000000, 0.000000000000000000, 1.000000000000000000 ) ) ;
#13340 = CARTESIAN_POINT ( 'NONE',  ( 66.02295749185039142, 31.67615731643408949, 4.000000000000000000 ) ) ;
#13341 = CARTESIAN_POINT ( 'NONE',  ( -14.40394475573012123, -13.79473832354794993, 16.99999999999999645 ) ) ;
#13342 = APPLICATION_PROTOCOL_DEFINITION ( 'draft international standard', 'automotive_design', 1998, #3900 ) ;
#13343 = CARTESIAN_POINT ( 'NONE',  ( 0.000000000000000000, 0.000000000000000000, 7.000000000000000000 ) ) ;
#13344 = VECTOR ( 'NONE', #6513, 1000.000000000000000 ) ;
#13345 = B_SPLINE_CURVE_WITH_KNOTS ( 'NONE', 3,
 ( #7302, #12121, #6219, #14683, #11972, #12209, #9758, #1460 ),
 .UNSPECIFIED., .F., .F.,
 ( 4, 2, 2, 4 ),
 ( 2.154797734452241992E-07, 0.001895231411414977432, 0.002842739377235738250, 0.003790247343056499067 ),
 .UNSPECIFIED. ) ;
#13346 = DIRECTION ( 'NONE',  ( 0.000000000000000000, 0.000000000000000000, 1.000000000000000000 ) ) ;
#13347 = DIRECTION ( 'NONE',  ( -1.000000000000000000, -0.000000000000000000, 0.000000000000000000 ) ) ;
#13348 = ORIENTED_EDGE ( 'NONE', *, *, #3697, .F. ) ;
#13349 = CARTESIAN_POINT ( 'NONE',  ( 75.68384697807671557, 11.35494834827056110, 7.000000000000000000 ) ) ;
#13350 = DIRECTION ( 'NONE',  ( -1.000000000000000000, 0.000000000000000000, 0.000000000000000000 ) ) ;
#13351 = CIRCLE ( 'NONE', #9919, 6.000000000000005329 ) ;
#13352 = CARTESIAN_POINT ( 'NONE',  ( -5.209999999999999964, 0.000000000000000000, 0.000000000000000000 ) ) ;
#13353 = ORIENTED_EDGE ( 'NONE', *, *, #13498, .T. ) ;
#13354 = TOROIDAL_SURFACE ( 'NONE', #83, 5.899999999999999467, 0.1000000000000010186 ) ;
#13355 = CIRCLE ( 'NONE', #11136, 2.524999999999999023 ) ;
#13356 = CARTESIAN_POINT ( 'NONE',  ( 2.765633920072234631, 5.391175441198615914, 24.15498966839965078 ) ) ;
#13357 = FACE_OUTER_BOUND ( 'NONE', #2238, .T. ) ;
#13358 = ORIENTED_EDGE ( 'NONE', *, *, #14900, .F. ) ;
#13359 = ORIENTED_EDGE ( 'NONE', *, *, #7322, .F. ) ;
#13360 = FACE_OUTER_BOUND ( 'NONE', #2743, .T. ) ;
#13361 = FACE_OUTER_BOUND ( 'NONE', #13187, .T. ) ;
#13362 = CARTESIAN_POINT ( 'NONE',  ( 0.1920563539683076970, -15.58455734132164316, -2.883512197589173542 ) ) ;
#13363 = LINE ( 'NONE', #9905, #1091 ) ;
#13364 = CARTESIAN_POINT ( 'NONE',  ( -5.209999999999999964, 0.000000000000000000, 0.000000000000000000 ) ) ;
#13365 = AXIS2_PLACEMENT_3D ( 'NONE', #12272, #10963, #4056 ) ;
#13366 = VECTOR ( 'NONE', #4645, 1000.000000000000000 ) ;
#13367 = AXIS2_PLACEMENT_3D ( 'NONE', #7571, #10096, #12483 ) ;
#13368 = CARTESIAN_POINT ( 'NONE',  ( 1.749999999999998002, 25.12109765559671004, -12.52377138324198391 ) ) ;
#13369 = ADVANCED_FACE ( 'NONE', ( #12052 ), #14163, .T. ) ;
#13370 = VERTEX_POINT ( 'NONE', #3841 ) ;
#13371 = DIRECTION ( 'NONE',  ( -1.000000000000000000, -0.000000000000000000, -0.000000000000000000 ) ) ;
#13372 = PRODUCT_DEFINITION_SHAPE ( 'NONE', 'NONE',  #1381 ) ;
#13373 = CARTESIAN_POINT ( 'NONE',  ( 2.789999999999999147, 13.68080036884355621, -5.229914364928207604 ) ) ;
#13374 = CIRCLE ( 'NONE', #614, 20.00000000000000000 ) ;
#13375 = SURFACE_SIDE_STYLE ('',( #13296 ) ) ;
#13376 = VECTOR ( 'NONE', #6926, 1000.000000000000114 ) ;
#13377 = ORIENTED_EDGE ( 'NONE', *, *, #10388, .F. ) ;
#13378 = ORIENTED_EDGE ( 'NONE', *, *, #4742, .T. ) ;
#13379 = VERTEX_POINT ( 'NONE', #2992 ) ;
#13380 = CARTESIAN_POINT ( 'NONE',  ( 1.039999999999997593, 0.000000000000000000, 0.000000000000000000 ) ) ;
#13381 = CARTESIAN_POINT ( 'NONE',  ( 33.82574562093736859, -6.697933970950280091, -2.000000000000000888 ) ) ;
#13382 = ORIENTED_EDGE ( 'NONE', *, *, #6985, .F. ) ;
#13383 = DIRECTION ( 'NONE',  ( -1.000000000000000000, -0.000000000000000000, -0.000000000000000000 ) ) ;
#13384 = TOROIDAL_SURFACE ( 'NONE', #11171, 14.01039946648074341, 8.000000000000000000 ) ;
#13385 = ORIENTED_EDGE ( 'NONE', *, *, #437, .T. ) ;
#13386 = AXIS2_PLACEMENT_3D ( 'NONE', #6786, #13852, #5651 ) ;
#13387 = LINE ( 'NONE', #12310, #13115 ) ;
#13388 = CARTESIAN_POINT ( 'NONE',  ( 8.000000000000000000, 0.000000000000000000, 0.000000000000000000 ) ) ;
#13389 = DIRECTION ( 'NONE',  ( 0.000000000000000000, 0.000000000000000000, 1.000000000000000000 ) ) ;
#13390 = EDGE_CURVE ( 'NONE', #613, #8861, #13217, .T. ) ;
#13391 = CARTESIAN_POINT ( 'NONE',  ( -3.799999999999999378, 4.653657836759941744E-16, 0.000000000000000000 ) ) ;
#13392 = DIRECTION ( 'NONE',  ( 0.000000000000000000, 1.374038396813314559E-15, -1.000000000000000000 ) ) ;
#13393 = MANIFOLD_SOLID_BREP ( 'Cut-Extrude2', #10399 ) ;
#13394 = EDGE_LOOP ( 'NONE', ( #9562, #311, #9043, #4734, #1727, #1355, #15183, #5252 ) ) ;
#13395 = CARTESIAN_POINT ( 'NONE',  ( 74.00000000000000000, 0.000000000000000000, 5.500000000000000000 ) ) ;
#13396 = VECTOR ( 'NONE', #4252, 1000.000000000000000 ) ;
#13397 = FACE_OUTER_BOUND ( 'NONE', #11896, .T. ) ;
#13398 = ORIENTED_EDGE ( 'NONE', *, *, #4695, .T. ) ;
#13399 = ORIENTED_EDGE ( 'NONE', *, *, #9029, .T. ) ;
#13400 = CARTESIAN_POINT ( 'NONE',  ( 0.000000000000000000, -24.04302995059967429, 1.991882183130232242 ) ) ;
#13401 = CARTESIAN_POINT ( 'NONE',  ( 1.749999999999998002, -25.12109765559663188, 12.52377138324213668 ) ) ;
#13402 = PRODUCT_RELATED_PRODUCT_CATEGORY ( 'part', '', ( #14394 ) ) ;
#13403 = EDGE_CURVE ( 'NONE', #11628, #11722, #2477, .T. ) ;
#13404 = EDGE_CURVE ( 'NONE', #8254, #14803, #6302, .T. ) ;
#13405 = CARTESIAN_POINT ( 'NONE',  ( 0.000000000000000000, 0.000000000000000000, 0.000000000000000000 ) ) ;
#13406 = FACE_BOUND ( 'NONE', #3956, .T. ) ;
#13407 = TOROIDAL_SURFACE ( 'NONE', #7766, 14.01039946648074341, 8.000000000000000000 ) ;
#13408 = DIRECTION ( 'NONE',  ( -0.000000000000000000, -0.000000000000000000, 1.000000000000000000 ) ) ;
#13409 = CIRCLE ( 'NONE', #10713, 17.95481323787947758 ) ;
#13410 = EDGE_LOOP ( 'NONE', ( #7612, #8497, #14432, #4209 ) ) ;
#13411 = CARTESIAN_POINT ( 'NONE',  ( -5.209999999999999964, 0.000000000000000000, 0.000000000000000000 ) ) ;
#13412 = CARTESIAN_POINT ( 'NONE',  ( 1.039999999999998037, 12.83329210556849276, -12.55714665599973756 ) ) ;
#13413 = CARTESIAN_POINT ( 'NONE',  ( 0.02436607992776151574, -18.55949924794880346, -16.37294372382878649 ) ) ;
#13414 = DIRECTION ( 'NONE',  ( -1.000000000000000000, -0.000000000000000000, 0.000000000000000000 ) ) ;
#13415 = ORIENTED_EDGE ( 'NONE', *, *, #7686, .T. ) ;
#13416 = EDGE_CURVE ( 'NONE', #12831, #1110, #6068, .T. ) ;
#13417 = ORIENTED_EDGE ( 'NONE', *, *, #10293, .F. ) ;
#13418 = EDGE_CURVE ( 'NONE', #2359, #4526, #7459, .T. ) ;
#13419 = ORIENTED_EDGE ( 'NONE', *, *, #4717, .F. ) ;
#13420 = CARTESIAN_POINT ( 'NONE',  ( 74.00000000000000000, 7.347880794884117764E-16, 7.000000000000000000 ) ) ;
#13421 = CARTESIAN_POINT ( 'NONE',  ( -14.40394475573012301, -4.794738323547945491, 16.99999999999999645 ) ) ;
#13422 = EDGE_CURVE ( 'NONE', #5333, #4276, #1616, .T. ) ;
#13423 = CARTESIAN_POINT ( 'NONE',  ( 33.82574562093736859, -6.697933970950280091, 2.999999999999999112 ) ) ;
#13424 = LINE ( 'NONE', #3978, #11157 ) ;
#13425 = SHAPE_DEFINITION_REPRESENTATION ( #7269, #2588 ) ;
#13426 = VECTOR ( 'NONE', #12880, 1000.000000000000000 ) ;
#13427 = FACE_OUTER_BOUND ( 'NONE', #8546, .T. ) ;
#13428 = AXIS2_PLACEMENT_3D ( 'NONE', #13287, #2841, #9988 ) ;
#13429 = CARTESIAN_POINT ( 'NONE',  ( 0.02436607992776151574, -18.55949924794880346, -16.37294372382878649 ) ) ;
#13430 = CARTESIAN_POINT ( 'NONE',  ( 74.00000000000000000, 7.347880794884121708E-16, 4.500000000000000888 ) ) ;
#13431 = EDGE_CURVE ( 'NONE', #9808, #10254, #3217, .T. ) ;
#13432 = ORIENTED_EDGE ( 'NONE', *, *, #3467, .T. ) ;
#13434 = AXIS2_PLACEMENT_3D ( 'NONE', #9479, #14177, #1329 ) ;
#13433 = CYLINDRICAL_SURFACE ( 'NONE', #708, 4.000000000000000000 ) ;
#13435 = FACE_OUTER_BOUND ( 'NONE', #1988, .T. ) ;
#13436 = DIRECTION ( 'NONE',  ( 0.000000000000000000, 0.000000000000000000, 1.000000000000000000 ) ) ;
#13437 = ORIENTED_EDGE ( 'NONE', *, *, #7270, .T. ) ;
#13438 = AXIS2_PLACEMENT_3D ( 'NONE', #1745, #12189, #8651 ) ;
#13439 = CARTESIAN_POINT ( 'NONE',  ( 0.5431870686475157584, -12.54666350726131618, 11.42270873787287933 ) ) ;
#13440 = DIRECTION ( 'NONE',  ( 1.000000000000000000, 0.000000000000000000, 0.000000000000000000 ) ) ;
#13441 = VERTEX_POINT ( 'NONE', #5171 ) ;
#13442 = TOROIDAL_SURFACE ( 'NONE', #7812, 14.01039946648073986, 8.000000000000000000 ) ;
#13443 = ORIENTED_EDGE ( 'NONE', *, *, #6891, .F. ) ;
#13444 =( LENGTH_UNIT ( ) NAMED_UNIT ( * ) SI_UNIT ( .MILLI., .METRE. ) );
#13445 = DIRECTION ( 'NONE',  ( -1.000000000000000000, -0.000000000000000000, -0.000000000000000000 ) ) ;
#13446 = CARTESIAN_POINT ( 'NONE',  ( 2.789999999999999147, -23.17675759782046541, 7.772527002114348882 ) ) ;
#13447 = CARTESIAN_POINT ( 'NONE',  ( 2.764680872513688659, 2.311161484776556030, 14.46287784598618309 ) ) ;
#13448 = DIRECTION ( 'NONE',  ( -0.9728364810787194505, -0.2314933715733012987, 0.000000000000000000 ) ) ;
#13449 = AXIS2_PLACEMENT_3D ( 'NONE', #6885, #10638, #11564 ) ;
#13450 = LINE ( 'NONE', #12057, #14728 ) ;
#13451 = ORIENTED_EDGE ( 'NONE', *, *, #3259, .T. ) ;
#13452 = FACE_OUTER_BOUND ( 'NONE', #11653, .T. ) ;
#13453 = CIRCLE ( 'NONE', #4866, 3.000000000000002665 ) ;
#13454 = VECTOR ( 'NONE', #4710, 1000.000000000000000 ) ;
#13455 = CARTESIAN_POINT ( 'NONE',  ( 101.6227766016837819, 5.204170427930421283E-15, 3.000000000000002665 ) ) ;
#13456 = VERTEX_POINT ( 'NONE', #9679 ) ;
#13457 = ORIENTED_EDGE ( 'NONE', *, *, #1586, .F. ) ;
#13458 = ORIENTED_EDGE ( 'NONE', *, *, #14949, .T. ) ;
#13459 = CARTESIAN_POINT ( 'NONE',  ( 1.394999999999999574, -24.89775460606841406, 12.96210679857778025 ) ) ;
#13460 = CARTESIAN_POINT ( 'NONE',  ( 2.601776121706765199, 17.47009390565519382, -19.18368891937472043 ) ) ;
#13461 = VERTEX_POINT ( 'NONE', #8667 ) ;
#13462 = AXIS2_PLACEMENT_3D ( 'NONE', #5173, #12290, #9839 ) ;
#13463 = VECTOR ( 'NONE', #12174, 1000.000000000000000 ) ;
#13464 = B_SPLINE_CURVE_WITH_KNOTS ( 'NONE', 3,
 ( #6081, #10768, #11132, #456, #6309, #14385 ),
 .UNSPECIFIED., .F., .F.,
 ( 4, 2, 4 ),
 ( 2.321268216997094965E-07, 0.001878622960950499009, 0.003757013795079297992 ),
 .UNSPECIFIED. ) ;
#13465 = ADVANCED_FACE ( 'NONE', ( #13360 ), #2839, .T. ) ;
#13466 = PRODUCT_DEFINITION_CONTEXT ( 'detailed design', #2034, 'design' ) ;
#13467 = DIRECTION ( 'NONE',  ( 0.000000000000000000, -0.4999999999999951705, -0.8660254037844413721 ) ) ;
#13468 = FACE_OUTER_BOUND ( 'NONE', #2854, .T. ) ;
#13469 = ORIENTED_EDGE ( 'NONE', *, *, #2163, .T. ) ;
#13470 = DIRECTION ( 'NONE',  ( 5.782411586589355667E-16, 1.000000000000000000, -0.000000000000000000 ) ) ;
#13471 = DIRECTION ( 'NONE',  ( 0.000000000000000000, 0.000000000000000000, 1.000000000000000000 ) ) ;
#13472 = DIRECTION ( 'NONE',  ( 0.4036950204470268200, -0.9148936170212768060, 0.000000000000000000 ) ) ;
#13473 = VECTOR ( 'NONE', #2893, 1000.000000000000000 ) ;
#13474 = AXIS2_PLACEMENT_3D ( 'NONE', #1864, #11151, #11940 ) ;
#13475 = DIRECTION ( 'NONE',  ( -1.000000000000000000, 0.000000000000000000, -0.000000000000000000 ) ) ;
#13476 = EDGE_CURVE ( 'NONE', #10133, #14329, #5236, .T. ) ;
#13477 = CARTESIAN_POINT ( 'NONE',  ( 2.764680872515354437, 13.68080036884355621, -5.229914364928207604 ) ) ;
#13478 = ORIENTED_EDGE ( 'NONE', *, *, #10571, .T. ) ;
#13479 = DIRECTION ( 'NONE',  ( 0.1643989873053570416, -0.9863939238321438596, 0.000000000000000000 ) ) ;
#13480 = ADVANCED_FACE ( 'NONE', ( #11583 ), #4229, .F. ) ;
#13481 = DIRECTION ( 'NONE',  ( 1.000000000000000000, 0.000000000000000000, 0.000000000000000000 ) ) ;
#13482 = ORIENTED_EDGE ( 'NONE', *, *, #11467, .T. ) ;
#13483 = ORIENTED_EDGE ( 'NONE', *, *, #10013, .T. ) ;
#13484 = CARTESIAN_POINT ( 'NONE',  ( -1.249999999999997558, 0.000000000000000000, 0.000000000000000000 ) ) ;
#13485 = DIRECTION ( 'NONE',  ( 1.000000000000000000, 0.000000000000000000, 0.000000000000000000 ) ) ;
#13486 = ADVANCED_FACE ( 'NONE', ( #10138 ), #763, .T. ) ;
#13487 = FILL_AREA_STYLE ('',( #9948 ) ) ;
#13488 = CARTESIAN_POINT ( 'NONE',  ( 4.000000000000000888, 4.898587196589413815E-16, -7.000000000000007994 ) ) ;
#13489 = CIRCLE ( 'NONE', #1212, 17.95481323787947403 ) ;
#13490 = CARTESIAN_POINT ( 'NONE',  ( 2.782650442329440921, -9.045126717605700861, -11.23191127083872942 ) ) ;
#13491 = VERTEX_POINT ( 'NONE', #2221 ) ;
#13492 = CARTESIAN_POINT ( 'NONE',  ( 2.789999999999999147, 24.44424927289185945, -0.2301004812058395077 ) ) ;
#13493 = CARTESIAN_POINT ( 'NONE',  ( -2.321707774797442170, -4.824281976789052351, -0.8000000000000000444 ) ) ;
#13494 = ORIENTED_EDGE ( 'NONE', *, *, #12184, .F. ) ;
#13495 = B_SPLINE_CURVE_WITH_KNOTS ( 'NONE', 3,
 ( #14749, #3280, #14817, #2127 ),
 .UNSPECIFIED., .F., .F.,
 ( 4, 4 ),
 ( 0.005258110598983609975, 0.005948376585272729597 ),
 .UNSPECIFIED. ) ;
#13496 = CARTESIAN_POINT ( 'NONE',  ( -19.40394475573012301, -7.794738323547950820, 14.99999999999999822 ) ) ;
#13497 = EDGE_CURVE ( 'NONE', #3044, #4505, #3948, .T. ) ;
#13498 = EDGE_CURVE ( 'NONE', #7299, #12118, #8262, .T. ) ;
#13499 = ORIENTED_EDGE ( 'NONE', *, *, #257, .T. ) ;
#13500 = AXIS2_PLACEMENT_3D ( 'NONE', #3747, #7598, #4997 ) ;
#13501 = ORIENTED_EDGE ( 'NONE', *, *, #13220, .T. ) ;
#13502 = ORIENTED_EDGE ( 'NONE', *, *, #14478, .T. ) ;
#13503 = CARTESIAN_POINT ( 'NONE',  ( -9.947158122877977619E-15, 13.12804621868830957, -5.226330906375914687 ) ) ;
#13504 = DIRECTION ( 'NONE',  ( 0.000000000000000000, 0.000000000000000000, 1.000000000000000000 ) ) ;
#13505 = DIRECTION ( 'NONE',  ( 0.000000000000000000, 0.000000000000000000, 1.000000000000000000 ) ) ;
#13506 = FACE_OUTER_BOUND ( 'NONE', #1670, .T. ) ;
#13507 = APPLICATION_PROTOCOL_DEFINITION ( 'draft international standard', 'automotive_design', 1998, #9197 ) ;
#13508 = CARTESIAN_POINT ( 'NONE',  ( 0.000000000000000000, 23.48180575137729775, 5.535312321042836103 ) ) ;
#13509 = PRODUCT ( 'connector', 'connector', '', ( #13576 ) ) ;
#13510 = CARTESIAN_POINT ( 'NONE',  ( -19.40394475573012301, -16.79473832354794993, 22.00000000000000000 ) ) ;
#13511 = DIRECTION ( 'NONE',  ( 0.000000000000000000, 0.000000000000000000, 1.000000000000000000 ) ) ;
#13512 = EDGE_CURVE ( 'NONE', #7983, #12618, #14174, .T. ) ;
#13513 = EDGE_LOOP ( 'NONE', ( #3370, #2705, #3526, #12051 ) ) ;
#13514 = DIRECTION ( 'NONE',  ( 0.000000000000000000, 0.000000000000000000, 1.000000000000000000 ) ) ;
#13515 = CARTESIAN_POINT ( 'NONE',  ( 2.765633920072238183, 2.336989772644269436, 24.63872515616083447 ) ) ;
#13516 = CARTESIAN_POINT ( 'NONE',  ( 0.02436607992776064838, 12.59161484032912171, 21.30679549418635688 ) ) ;
#13517 = ADVANCED_FACE ( 'NONE', ( #3293 ), #7755, .F. ) ;
#13518 = ADVANCED_FACE ( 'NONE', ( #11430 ), #13684, .T. ) ;
#13519 = ORIENTED_EDGE ( 'NONE', *, *, #4266, .T. ) ;
#13520 = DIRECTION ( 'NONE',  ( 0.000000000000000000, 0.000000000000000000, 1.000000000000000000 ) ) ;
#13521 = CARTESIAN_POINT ( 'NONE',  ( 1.749999999999998002, 24.89775460606832524, 12.96210679857795256 ) ) ;
#13522 = ORIENTED_EDGE ( 'NONE', *, *, #4495, .F. ) ;
#13523 = ORIENTED_EDGE ( 'NONE', *, *, #6055, .F. ) ;
#13524 = SURFACE_SIDE_STYLE ('',( #2698 ) ) ;
#13525 = FACE_OUTER_BOUND ( 'NONE', #11398, .T. ) ;
#13526 = CARTESIAN_POINT ( 'NONE',  ( 2.789999999999999147, 8.624777288397954322, -11.04103753892262496 ) ) ;
#13527 = DIRECTION ( 'NONE',  ( -1.000000000000000000, -0.000000000000000000, -0.000000000000000000 ) ) ;
#13528 = CARTESIAN_POINT ( 'NONE',  ( 1.039999999999997593, 0.000000000000000000, 0.000000000000000000 ) ) ;
#13529 = CARTESIAN_POINT ( 'NONE',  ( 2.031033491000349134, 24.80232951178394885, -12.05173163741697451 ) ) ;
#13530 = B_SPLINE_CURVE_WITH_KNOTS ( 'NONE', 3,
 ( #765, #10141, #14832, #3230 ),
 .UNSPECIFIED., .F., .F.,
 ( 4, 4 ),
 ( 2.159563976928984569E-07, 0.0006916893629249152697 ),
 .UNSPECIFIED. ) ;
#13531 = ORIENTED_EDGE ( 'NONE', *, *, #3116, .F. ) ;
#13532 = DIRECTION ( 'NONE',  ( -0.000000000000000000, -0.000000000000000000, 1.000000000000000000 ) ) ;
#13533 = DIRECTION ( 'NONE',  ( 1.000000000000000000, 0.000000000000000000, 0.000000000000000000 ) ) ;
#13534 = ORIENTED_EDGE ( 'NONE', *, *, #742, .T. ) ;
#13535 = PRESENTATION_STYLE_ASSIGNMENT (( #1705 ) ) ;
#13536 = ORIENTED_EDGE ( 'NONE', *, *, #14074, .T. ) ;
#13537 = ORIENTED_EDGE ( 'NONE', *, *, #4266, .F. ) ;
#13538 = ORIENTED_EDGE ( 'NONE', *, *, #1484, .T. ) ;
#13539 = LINE ( 'NONE', #13459, #5061 ) ;
#13540 = AXIS2_PLACEMENT_3D ( 'NONE', #8932, #786, #12613 ) ;
#13541 = EDGE_CURVE ( 'NONE', #7400, #11004, #10006, .T. ) ;
#13542 = CARTESIAN_POINT ( 'NONE',  ( 4.424224194511527805E-17, 20.65025570340106853, -12.51972505884970488 ) ) ;
#13543 = CARTESIAN_POINT ( 'NONE',  ( 1.394999999999998685, 12.55714665599987079, 12.83329210556836308 ) ) ;
#13544 = EDGE_LOOP ( 'NONE', ( #9817, #11375 ) ) ;
#13545 = FACE_OUTER_BOUND ( 'NONE', #2256, .T. ) ;
#13546 = CARTESIAN_POINT ( 'NONE',  ( 4.000000000000000000, 4.898587196589412829E-16, 6.000000000000000000 ) ) ;
#13547 = DIRECTION ( 'NONE',  ( -1.000000000000000000, -0.000000000000000000, -0.000000000000000000 ) ) ;
#13548 = ADVANCED_FACE ( 'NONE', ( #5537 ), #1923, .T. ) ;
#13549 = ORIENTED_EDGE ( 'NONE', *, *, #10773, .T. ) ;
#13550 = B_SPLINE_CURVE_WITH_KNOTS ( 'NONE', 3,
 ( #4814, #90, #8255, #9567, #11785, #3347, #2496, #2201 ),
 .UNSPECIFIED., .F., .F.,
 ( 4, 2, 2, 4 ),
 ( 2.445728210282435608E-07, 0.001895260649874691344, 0.002842768688401522276, 0.003790276726928352991 ),
 .UNSPECIFIED. ) ;
#13551 = LINE ( 'NONE', #2953, #9980 ) ;
#13552 = CARTESIAN_POINT ( 'NONE',  ( 2.789999999999999147, -12.52067188844336165, -20.62201879784926462 ) ) ;
#13553 = ORIENTED_EDGE ( 'NONE', *, *, #11610, .T. ) ;
#13554 = ORIENTED_EDGE ( 'NONE', *, *, #12465, .T. ) ;
#13555 = LINE ( 'NONE', #1963, #1934 ) ;
#13556 = CIRCLE ( 'NONE', #7182, 24.12539914357697413 ) ;
#13557 = AXIS2_PLACEMENT_3D ( 'NONE', #12561, #4201, #8870 ) ;
#13558 = FILL_AREA_STYLE_COLOUR ( '', #14176 ) ;
#13559 = CARTESIAN_POINT ( 'NONE',  ( 0.1855655959470664251, -17.45907811351468553, 19.17825124759772493 ) ) ;
#13560 = EDGE_CURVE ( 'NONE', #7568, #13720, #11291, .T. ) ;
#13561 = ORIENTED_EDGE ( 'NONE', *, *, #10613, .T. ) ;
#13562 = DIRECTION ( 'NONE',  ( -0.9728364810787194505, -0.2314933715733012987, 0.000000000000000000 ) ) ;
#13563 = EDGE_CURVE ( 'NONE', #14234, #446, #3136, .T. ) ;
#13564 = ORIENTED_EDGE ( 'NONE', *, *, #9173, .F. ) ;
#13565 = DIRECTION ( 'NONE',  ( -1.000000000000000000, -0.000000000000000000, -0.000000000000000000 ) ) ;
#13566 = DIRECTION ( 'NONE',  ( 0.000000000000000000, 0.000000000000000000, -1.000000000000000000 ) ) ;
#13567 = ORIENTED_EDGE ( 'NONE', *, *, #3248, .T. ) ;
#13568 = CARTESIAN_POINT ( 'NONE',  ( 70.16198417812034904, 9.730076655429538590, 7.000000000000000000 ) ) ;
#13569 = FACE_OUTER_BOUND ( 'NONE', #5083, .T. ) ;
#13570 = ORIENTED_EDGE ( 'NONE', *, *, #876, .F. ) ;
#13571 = ORIENTED_EDGE ( 'NONE', *, *, #9349, .F. ) ;
#13572 = ORIENTED_EDGE ( 'NONE', *, *, #13116, .T. ) ;
#13573 = CARTESIAN_POINT ( 'NONE',  ( -4.000000000000000000, 0.000000000000000000, 3.895000000000000462 ) ) ;
#13574 = CARTESIAN_POINT ( 'NONE',  ( 4.000000000000000000, 4.898587196589412829E-16, 3.895000000000000462 ) ) ;
#13575 = CARTESIAN_POINT ( 'NONE',  ( 0.02531912748679129854, 11.36963888406687317, 9.232963481057801403 ) ) ;
#13576 = PRODUCT_CONTEXT ( 'NONE', #9197, 'mechanical' ) ;
#13577 = CARTESIAN_POINT ( 'NONE',  ( 0.1920562174424405855, -10.28947301956291049, 12.05486625177567994 ) ) ;
#13578 = CARTESIAN_POINT ( 'NONE',  ( 0.000000000000000000, 5.535312321042724193, 23.48180575137730841 ) ) ;
#13579 = DIRECTION ( 'NONE',  ( 1.000000000000000000, 0.000000000000000000, 0.000000000000000000 ) ) ;
#13580 = ORIENTED_EDGE ( 'NONE', *, *, #2445, .T. ) ;
#13581 = CARTESIAN_POINT ( 'NONE',  ( 83.50748565343083385, 13.38500995229612478, -2.000000000000000888 ) ) ;
#13582 = CYLINDRICAL_SURFACE ( 'NONE', #13797, 28.06981291497571362 ) ;
#13583 = DIRECTION ( 'NONE',  ( 0.000000000000000000, 1.000000000000000000, -1.224646799147353207E-16 ) ) ;
#13584 = EDGE_LOOP ( 'NONE', ( #8146, #8430, #10169, #4 ) ) ;
#13585 = EDGE_CURVE ( 'NONE', #14933, #10147, #12179, .T. ) ;
#13586 = PLANE ( 'NONE',  #2608 ) ;
#13587 = LINE ( 'NONE', #6609, #10704 ) ;
#13588 = ORIENTED_EDGE ( 'NONE', *, *, #3917, .F. ) ;
#13589 = ORIENTED_EDGE ( 'NONE', *, *, #1484, .F. ) ;
#13590 = CARTESIAN_POINT ( 'NONE',  ( 0.7686372590627846835, 5.021526291670549647, -16.74220655292932136 ) ) ;
#13591 = CYLINDRICAL_SURFACE ( 'NONE', #13687, 3.000000000000002665 ) ;
#13592 = CARTESIAN_POINT ( 'NONE',  ( 0.006974657972266078837, 5.408388659524427489, -23.92335783895632417 ) ) ;
#13593 = PLANE ( 'NONE',  #10910 ) ;
#13594 = CARTESIAN_POINT ( 'NONE',  ( 0.02436607992775978102, 24.63872515616082737, 2.336989772644355146 ) ) ;
#13595 = ADVANCED_FACE ( 'NONE', ( #1998 ), #6681, .T. ) ;
#13596 = EDGE_CURVE ( 'NONE', #807, #14075, #5110, .T. ) ;
#13597 = DIRECTION ( 'NONE',  ( 1.000000000000000000, 0.000000000000000000, 0.000000000000000000 ) ) ;
#13598 = CARTESIAN_POINT ( 'NONE',  ( 0.5279273746168616777, 26.57710921259767645, -4.996265754456091557 ) ) ;
#13599 = ORIENTED_EDGE ( 'NONE', *, *, #6293, .T. ) ;
#13600 = CARTESIAN_POINT ( 'NONE',  ( 2.740003288479521792, 14.75565684666127098, 2.439987328297021918 ) ) ;
#13601 = VECTOR ( 'NONE', #12077, 1000.000000000000000 ) ;
#13602 = AXIS2_PLACEMENT_3D ( 'NONE', #10632, #82, #4808 ) ;
#13603 = FACE_OUTER_BOUND ( 'NONE', #265, .T. ) ;
#13604 = CIRCLE ( 'NONE', #14588, 5.000000000000000888 ) ;
#13605 = EDGE_LOOP ( 'NONE', ( #4874, #14411, #2724, #11019, #14864, #2764, #12609 ) ) ;
#13606 = ORIENTED_EDGE ( 'NONE', *, *, #5595, .T. ) ;
#13607 = VERTEX_POINT ( 'NONE', #4917 ) ;
#13608 = ORIENTED_EDGE ( 'NONE', *, *, #2445, .F. ) ;
#13609 = EDGE_CURVE ( 'NONE', #12348, #2656, #5912, .T. ) ;
#13610 = CARTESIAN_POINT ( 'NONE',  ( -10.00000000000000000, 0.000000000000000000, 0.000000000000000000 ) ) ;
#13611 = CIRCLE ( 'NONE', #841, 14.01039946648073986 ) ;
#13612 = EDGE_CURVE ( 'NONE', #8808, #1432, #12805, .T. ) ;
#13613 = CARTESIAN_POINT ( 'NONE',  ( 0.000000000000000000, 7.909232158575156824, -24.34211360614291664 ) ) ;
#13614 = VECTOR ( 'NONE', #4161, 1000.000000000000000 ) ;
#13615 = ADVANCED_FACE ( 'NONE', ( #10524 ), #10591, .F. ) ;
#13616 = CARTESIAN_POINT ( 'NONE',  ( 4.000000000000000888, 4.898587196589413815E-16, 10.00000000000000000 ) ) ;
#13617 = CARTESIAN_POINT ( 'NONE',  ( 69.97572749000833880, 15.55805301486455683, 2.999999999999999112 ) ) ;
#13618 = ORIENTED_EDGE ( 'NONE', *, *, #3133, .T. ) ;
#13619 = FACE_OUTER_BOUND ( 'NONE', #8030, .T. ) ;
#13620 = CYLINDRICAL_SURFACE ( 'NONE', #3877, 2.524999999999999467 ) ;
#13621 = AXIS2_PLACEMENT_3D ( 'NONE', #13196, #352, #1748 ) ;
#13622 = EDGE_CURVE ( 'NONE', #1439, #12007, #1001, .T. ) ;
#13623 = CARTESIAN_POINT ( 'NONE',  ( 62.65957446808508280, 26.91300136313512326, 4.000000000000001776 ) ) ;
#13624 = VECTOR ( 'NONE', #11472, 1000.000000000000000 ) ;
#13625 = DIRECTION ( 'NONE',  ( -1.000000000000000000, 0.000000000000000000, 0.000000000000000000 ) ) ;
#13626 = VERTEX_POINT ( 'NONE', #14203 ) ;
#13627 = LINE ( 'NONE', #3108, #15151 ) ;
#13628 = CARTESIAN_POINT ( 'NONE',  ( 0.000000000000000000, 12.98979500319694225, 5.249430348645796940 ) ) ;
#13629 = ORIENTED_EDGE ( 'NONE', *, *, #5323, .F. ) ;
#13630 = ORIENTED_EDGE ( 'NONE', *, *, #14002, .F. ) ;
#13632 = DIRECTION ( 'NONE',  ( -1.000000000000000000, -0.000000000000000000, -0.000000000000000000 ) ) ;
#13631 = AXIS2_PLACEMENT_3D ( 'NONE', #3413, #12841, #10482 ) ;
#13633 = AXIS2_PLACEMENT_3D ( 'NONE', #15008, #6775, #3094 ) ;
#13634 = SHAPE_REPRESENTATION_RELATIONSHIP ( 'NONE' , 'NONE' ,  #10044, #4912 ) ;
#13635 = DIRECTION ( 'NONE',  ( 0.000000000000000000, 0.000000000000000000, 1.000000000000000000 ) ) ;
#13636 = ORIENTED_EDGE ( 'NONE', *, *, #4509, .F. ) ;
#13637 = DIRECTION ( 'NONE',  ( 0.000000000000000000, 0.000000000000000000, 1.000000000000000000 ) ) ;
#13638 = EDGE_LOOP ( 'NONE', ( #8207, #7244, #13875, #7770 ) ) ;
#13639 = CARTESIAN_POINT ( 'NONE',  ( 0.02436607992776064838, 18.55949924794892780, 16.37294372382865504 ) ) ;
#13640 = DIRECTION ( 'NONE',  ( 0.000000000000000000, 0.000000000000000000, 1.000000000000000000 ) ) ;
#13641 = EDGE_LOOP ( 'NONE', ( #1298, #874, #2523, #2397, #3940, #7909 ) ) ;
#13642 = ADVANCED_FACE ( 'NONE', ( #15221 ), #4754, .F. ) ;
#13643 = AXIS2_PLACEMENT_3D ( 'NONE', #11207, #13440, #12210 ) ;
#13644 =( NAMED_UNIT ( * ) PLANE_ANGLE_UNIT ( ) SI_UNIT ( $, .RADIAN. ) );
#13645 = CARTESIAN_POINT ( 'NONE',  ( 2.601776105308175602, -25.78859396478526023, -2.857713464478961463 ) ) ;
#13646 = EDGE_LOOP ( 'NONE', ( #1025, #5106, #10581, #3779, #10172, #11873, #1129, #69, #3578, #11229, #6994, #14505 ) ) ;
#13647 = VERTEX_POINT ( 'NONE', #4690 ) ;
#13648 = DIRECTION ( 'NONE',  ( 0.000000000000000000, 0.000000000000000000, 1.000000000000000000 ) ) ;
#13649 = CARTESIAN_POINT ( 'NONE',  ( 2.700841271786576403, -14.29252738795474720, 5.279841123860291141 ) ) ;
#13650 = AXIS2_PLACEMENT_3D ( 'NONE', #15150, #6066, #9522 ) ;
#13651 = DIRECTION ( 'NONE',  ( -0.000000000000000000, -0.000000000000000000, 1.000000000000000000 ) ) ;
#13652 = LINE ( 'NONE', #7822, #9931 ) ;
#13653 =( NAMED_UNIT ( * ) PLANE_ANGLE_UNIT ( ) SI_UNIT ( $, .RADIAN. ) );
#13654 = DIRECTION ( 'NONE',  ( 0.000000000000000000, 0.000000000000000000, -1.000000000000000000 ) ) ;
#13655 = AXIS2_PLACEMENT_3D ( 'NONE', #5750, #1563, #8475 ) ;
#13656 = CARTESIAN_POINT ( 'NONE',  ( 2.789999999999999147, 1.991882183130632589, -24.04302995059963877 ) ) ;
#13657 = DIRECTION ( 'NONE',  ( 0.000000000000000000, 0.000000000000000000, 1.000000000000000000 ) ) ;
#13658 = VERTEX_POINT ( 'NONE', #13978 ) ;
#13659 = PLANE ( 'NONE',  #2180 ) ;
#13660 = CARTESIAN_POINT ( 'NONE',  ( -0.2000000000000000111, -6.997142273814360713, -0.8000000000000000444 ) ) ;
#13661 = CARTESIAN_POINT ( 'NONE',  ( 2.789999999999999147, -12.59161484032896361, -21.30679549418645280 ) ) ;
#13662 = CIRCLE ( 'NONE', #9005, 14.01039946648073986 ) ;
#13663 = CIRCLE ( 'NONE', #7035, 4.000000000000000000 ) ;
#13664 = ORIENTED_EDGE ( 'NONE', *, *, #10110, .T. ) ;
#13665 = DIRECTION ( 'NONE',  ( 0.000000000000000000, 1.224646799147353207E-16, 1.000000000000000000 ) ) ;
#13666 = CARTESIAN_POINT ( 'NONE',  ( -5.209999999999999964, 0.000000000000000000, 0.000000000000000000 ) ) ;
#13667 = EDGE_LOOP ( 'NONE', ( #4318, #9538, #3005, #14221, #1522, #13451, #2956, #568, #3553, #1836, #13483, #12559, #10681, #6515, #14627, #5495, #11907, #12086, #9507, #1687, #4880, #2484, #10, #9780, #12839 ) ) ;
#13668 = AXIS2_PLACEMENT_3D ( 'NONE', #4856, #6996, #4707 ) ;
#13669 = CIRCLE ( 'NONE', #7086, 3.000000000000000888 ) ;
#13670 = ORIENTED_EDGE ( 'NONE', *, *, #15215, .F. ) ;
#13671 = AXIS2_PLACEMENT_3D ( 'NONE', #7821, #2121, #6593 ) ;
#13672 = DIRECTION ( 'NONE',  ( 0.000000000000000000, 0.000000000000000000, -1.000000000000000000 ) ) ;
#13673 = CARTESIAN_POINT ( 'NONE',  ( 2.789999999999999147, -15.04425356660744839, -18.18163861606288378 ) ) ;
#13674 = ADVANCED_FACE ( 'NONE', ( #9359 ), #7281, .T. ) ;
#13675 = DIRECTION ( 'NONE',  ( -1.000000000000000000, -0.000000000000000000, -0.000000000000000000 ) ) ;
#13676 = CYLINDRICAL_SURFACE ( 'NONE', #1323, 17.95481323787947403 ) ;
#13677 = CARTESIAN_POINT ( 'NONE',  ( 0.02436607992776238310, -12.59161484032927092, 21.30679549418627161 ) ) ;
#13678 = AXIS2_PLACEMENT_3D ( 'NONE', #8952, #7887, #5374 ) ;
#13679 = EDGE_CURVE ( 'NONE', #12512, #316, #12926, .T. ) ;
#13680 = DIRECTION ( 'NONE',  ( -1.000000000000000000, -0.000000000000000000, -0.000000000000000000 ) ) ;
#13681 = CARTESIAN_POINT ( 'NONE',  ( 93.63799900313688340, -2.337932895214617890, 4.000000000000000000 ) ) ;
#13682 = ORIENTED_EDGE ( 'NONE', *, *, #10218, .F. ) ;
#13683 = CARTESIAN_POINT ( 'NONE',  ( 0.000000000000000000, 24.04302995059966364, -1.991882183130399664 ) ) ;
#13684 = TOROIDAL_SURFACE ( 'NONE', #5596, 14.01039946648074341, 8.000000000000000000 ) ;
#13685 = CIRCLE ( 'NONE', #14438, 28.06981291497571007 ) ;
#13686 = CARTESIAN_POINT ( 'NONE',  ( 2.789999999999999147, -11.04103753892277417, 8.624777288397760699 ) ) ;
#13687 = AXIS2_PLACEMENT_3D ( 'NONE', #10067, #11062, #7460 ) ;
#13688 = EDGE_LOOP ( 'NONE', ( #7150, #13564, #5026, #13798 ) ) ;
#13689 = AXIS2_PLACEMENT_3D ( 'NONE', #13326, #6120, #9643 ) ;
#13690 = B_SPLINE_CURVE_WITH_KNOTS ( 'NONE', 3,
 ( #4923, #9366, #2295, #5917, #11743, #13037 ),
 .UNSPECIFIED., .F., .F.,
 ( 4, 2, 4 ),
 ( 2.132675795045741476E-07, 0.001878604073277002386, 0.003756994878974500435 ),
 .UNSPECIFIED. ) ;
#13691 = EDGE_CURVE ( 'NONE', #13251, #7858, #3018, .T. ) ;
#13692 = EDGE_CURVE ( 'NONE', #9808, #14563, #6320, .T. ) ;
#13693 = ORIENTED_EDGE ( 'NONE', *, *, #2983, .T. ) ;
#13694 = ORIENTED_EDGE ( 'NONE', *, *, #5278, .F. ) ;
#13695 = ORIENTED_EDGE ( 'NONE', *, *, #13139, .F. ) ;
#13696 = CARTESIAN_POINT ( 'NONE',  ( 2.337784053193427969, -12.42068120944088605, 11.13074453164198729 ) ) ;
#13697 = CARTESIAN_POINT ( 'NONE',  ( 72.68384697807672978, 11.35494834827056110, 6.000000000000000000 ) ) ;
#13698 = AXIS2_PLACEMENT_3D ( 'NONE', #10766, #1468, #9682 ) ;
#13699 = AXIS2_PLACEMENT_3D ( 'NONE', #3741, #7202, #2449 ) ;
#13700 = CARTESIAN_POINT ( 'NONE',  ( 0.000000000000000000, -13.87420763704360382, -1.948757464274321949 ) ) ;
#13701 = ORIENTED_EDGE ( 'NONE', *, *, #3452, .F. ) ;
#13702 = CARTESIAN_POINT ( 'NONE',  ( 2.789999999999999147, 9.324097380959445402, 22.25075486061742325 ) ) ;
#13703 = DIRECTION ( 'NONE',  ( 0.000000000000000000, 0.000000000000000000, 1.000000000000000000 ) ) ;
#13704 = EDGE_CURVE ( 'NONE', #3376, #1316, #5774, .T. ) ;
#13705 = DIRECTION ( 'NONE',  ( 0.000000000000000000, 0.000000000000000000, 1.000000000000000000 ) ) ;
#13706 = CIRCLE ( 'NONE', #7819, 28.06981291497571007 ) ;
#13707 = CARTESIAN_POINT ( 'NONE',  ( -19.40394475573012301, -7.794738323547950820, 14.99999999999999822 ) ) ;
#13708 = ADVANCED_FACE ( 'NONE', ( #1279 ), #2647, .T. ) ;
#13709 = TOROIDAL_SURFACE ( 'NONE', #2801, 24.12539914357697768, 8.000000000000000000 ) ;
#13710 = AXIS2_PLACEMENT_3D ( 'NONE', #13411, #7430, #2889 ) ;
#13711 = ORIENTED_EDGE ( 'NONE', *, *, #14741, .T. ) ;
#13712 = DIRECTION ( 'NONE',  ( 0.000000000000000000, 0.000000000000000000, 1.000000000000000000 ) ) ;
#13713 = DIRECTION ( 'NONE',  ( -0.000000000000000000, -0.000000000000000000, 1.000000000000000000 ) ) ;
#13714 = B_SPLINE_CURVE_WITH_KNOTS ( 'NONE', 3,
 ( #8721, #339, #2742, #2894 ),
 .UNSPECIFIED., .F., .F.,
 ( 4, 4 ),
 ( 0.005258110598983608240, 0.005948376585272733934 ),
 .UNSPECIFIED. ) ;
#13715 = ORIENTED_EDGE ( 'NONE', *, *, #10181, .T. ) ;
#13716 = VERTEX_POINT ( 'NONE', #111 ) ;
#13717 = EDGE_CURVE ( 'NONE', #2934, #1779, #13029, .T. ) ;
#13718 = SURFACE_STYLE_USAGE ( .BOTH. , #4426 ) ;
#13719 = CARTESIAN_POINT ( 'NONE',  ( 75.20570977803312473, 12.97982004111159959, 2.999999999999999112 ) ) ;
#13720 = VERTEX_POINT ( 'NONE', #197 ) ;
#13721 = DIRECTION ( 'NONE',  ( -1.000000000000000000, 0.000000000000000000, 0.000000000000000000 ) ) ;
#13722 = CIRCLE ( 'NONE', #7590, 14.01039946648073986 ) ;
#13723 = CIRCLE ( 'NONE', #5113, 2.524999999999995470 ) ;
#13724 = VERTEX_POINT ( 'NONE', #9586 ) ;
#13725 = CARTESIAN_POINT ( 'NONE',  ( 2.765633920072235519, 9.836394144776026138, -22.71065055754441531 ) ) ;
#13726 = CARTESIAN_POINT ( 'NONE',  ( 0.01273908760111100436, -13.49730943211464762, -5.214906618940456262 ) ) ;
#13727 = VERTEX_POINT ( 'NONE', #3740 ) ;
#13728 = CARTESIAN_POINT ( 'NONE',  ( 1.666666666666673624, 0.000000000000000000, 4.000000000000003553 ) ) ;
#13729 = CARTESIAN_POINT ( 'NONE',  ( 2.789999999999999147, -11.07980565117287242, 9.999777909379893970 ) ) ;
#13730 = VERTEX_POINT ( 'NONE', #8418 ) ;
#13731 = VERTEX_POINT ( 'NONE', #11040 ) ;
#13732 = DIRECTION ( 'NONE',  ( 0.000000000000000000, 0.000000000000000000, 1.000000000000000000 ) ) ;
#13733 = AXIS2_PLACEMENT_3D ( 'NONE', #6860, #14942, #6779 ) ;
#13734 = CARTESIAN_POINT ( 'NONE',  ( -14.40394475573011945, -10.79473832354794460, -3.000000000000000000 ) ) ;
#13735 = ADVANCED_FACE ( 'NONE', ( #1513 ), #5217, .F. ) ;
#13736 = DIRECTION ( 'NONE',  ( 1.576560579138138762E-17, -1.359337748750801608E-17, 1.000000000000000000 ) ) ;
#13737 = PLANE ( 'NONE',  #8955 ) ;
#13738 = CARTESIAN_POINT ( 'NONE',  ( 0.7795480763126767521, -11.98750039041503257, 12.70439593876656481 ) ) ;
#13739 = FACE_OUTER_BOUND ( 'NONE', #8036, .T. ) ;
#13740 = ORIENTED_EDGE ( 'NONE', *, *, #3814, .F. ) ;
#13741 = DIRECTION ( 'NONE',  ( -1.000000000000000000, -0.000000000000000000, -0.000000000000000000 ) ) ;
#13742 = FACE_OUTER_BOUND ( 'NONE', #7901, .T. ) ;
#13743 = CIRCLE ( 'NONE', #6638, 2.999999999999988898 ) ;
#13744 = DIRECTION ( 'NONE',  ( 0.000000000000000000, 1.224646799147351975E-16, 1.000000000000000000 ) ) ;
#13745 = ORIENTED_EDGE ( 'NONE', *, *, #434, .T. ) ;
#13746 = EDGE_CURVE ( 'NONE', #1373, #3861, #11264, .T. ) ;
#13747 = DIRECTION ( 'NONE',  ( 1.000000000000000000, 0.000000000000000000, 0.000000000000000000 ) ) ;
#13748 = CARTESIAN_POINT ( 'NONE',  ( 0.000000000000000000, -12.98979500319690850, -5.249430348645889310 ) ) ;
#13749 = ORIENTED_EDGE ( 'NONE', *, *, #6352, .T. ) ;
#13750 = VERTEX_POINT ( 'NONE', #10813 ) ;
#13751 = DIRECTION ( 'NONE',  ( 0.000000000000000000, 0.000000000000000000, 1.000000000000000000 ) ) ;
#13752 = DIRECTION ( 'NONE',  ( 2.081668171172168513E-16, -1.000000000000000000, 0.000000000000000000 ) ) ;
#13753 = EDGE_LOOP ( 'NONE', ( #6294, #2514 ) ) ;
#13754 = DIRECTION ( 'NONE',  ( 0.000000000000000000, 0.000000000000000000, 1.000000000000000000 ) ) ;
#13755 = LINE ( 'NONE', #6759, #8206 ) ;
#13756 = CIRCLE ( 'NONE', #3208, 4.000000000000000000 ) ;
#13757 = DIRECTION ( 'NONE',  ( -0.9873505073845698643, 0.1585527532634883330, -5.103307673902845341E-17 ) ) ;
#13758 = CARTESIAN_POINT ( 'NONE',  ( 2.789999999999999147, -18.28042085475289369, 15.74360496233375173 ) ) ;
#13759 = CARTESIAN_POINT ( 'NONE',  ( 2.430066721642811345, 23.15620303736532293, 12.90954937922509238 ) ) ;
#13760 = EDGE_CURVE ( 'NONE', #4864, #3461, #3816, .T. ) ;
#13761 = VERTEX_POINT ( 'NONE', #14439 ) ;
#13762 = CARTESIAN_POINT ( 'NONE',  ( -19.40394475573012301, -7.794738323547950820, 14.99999999999999822 ) ) ;
#13763 = CARTESIAN_POINT ( 'NONE',  ( 2.789999999999999147, -1.948757464274269102, 13.87420763704360560 ) ) ;
#13764 = EDGE_CURVE ( 'NONE', #5744, #4588, #11536, .T. ) ;
#13765 = EDGE_LOOP ( 'NONE', ( #14486, #5848, #8523, #10556 ) ) ;
#13766 = SHAPE_REPRESENTATION_RELATIONSHIP ( 'NONE' , 'NONE' ,  #14263, #1226 ) ;
#13767 = B_SPLINE_CURVE_WITH_KNOTS ( 'NONE', 3,
 ( #11782, #5951, #12783, #2267, #12853, #6953 ),
 .UNSPECIFIED., .F., .F.,
 ( 4, 2, 4 ),
 ( 4.462636808935014747E-07, 0.001879885123572234236, 0.003759323983463574645 ),
 .UNSPECIFIED. ) ;
#13768 = EDGE_LOOP ( 'NONE', ( #10845, #4700 ) ) ;
#13769 = EDGE_LOOP ( 'NONE', ( #13399, #2899 ) ) ;
#13770 = ORIENTED_EDGE ( 'NONE', *, *, #5658, .T. ) ;
#13771 = CARTESIAN_POINT ( 'NONE',  ( 2.765633920072235963, 24.63872515616082737, 2.336989772644355146 ) ) ;
#13772 = DIRECTION ( 'NONE',  ( 1.000000000000000000, 0.000000000000000000, 0.000000000000000000 ) ) ;
#13773 = CARTESIAN_POINT ( 'NONE',  ( 1.394999999999999574, -27.76164181293054511, 4.147968289691193355 ) ) ;
#13774 = ADVANCED_FACE ( 'NONE', ( #6278 ), #8275, .T. ) ;
#13775 = EDGE_LOOP ( 'NONE', ( #3804, #6192, #10491, #8247 ) ) ;
#13776 = DIRECTION ( 'NONE',  ( -0.000000000000000000, -0.000000000000000000, -1.000000000000000000 ) ) ;
#13777 = DIRECTION ( 'NONE',  ( -0.9148936170212769170, -0.4036950204470268200, 0.000000000000000000 ) ) ;
#13778 = CARTESIAN_POINT ( 'NONE',  ( -9.999999999999998224, -1.390791565672605534, 4.000000000000003553 ) ) ;
#13779 = EDGE_CURVE ( 'NONE', #6121, #1565, #922, .T. ) ;
#13780 = VERTEX_POINT ( 'NONE', #4053 ) ;
#13781 = DIRECTION ( 'NONE',  ( 0.000000000000000000, 0.000000000000000000, -1.000000000000000000 ) ) ;
#13782 = DIRECTION ( 'NONE',  ( -0.5416238976136773520, 0.8406209333187989463, 0.000000000000000000 ) ) ;
#13783 = ORIENTED_EDGE ( 'NONE', *, *, #13166, .F. ) ;
#13784 = VERTEX_POINT ( 'NONE', #13338 ) ;
#13785 = ADVANCED_FACE ( 'NONE', ( #5294 ), #8582, .T. ) ;
#13786 = CARTESIAN_POINT ( 'NONE',  ( 1.039999999999997593, 0.000000000000000000, 0.000000000000000000 ) ) ;
#13787 = EDGE_CURVE ( 'NONE', #1778, #14991, #6204, .T. ) ;
#13788 = EDGE_CURVE ( 'NONE', #12141, #10760, #14844, .T. ) ;
#13789 = EDGE_LOOP ( 'NONE', ( #13378, #5943, #5453, #12739 ) ) ;
#13790 = CARTESIAN_POINT ( 'NONE',  ( 2.789999999999999147, 22.25075486061738772, 9.324097380959527115 ) ) ;
#13791 = B_SPLINE_CURVE_WITH_KNOTS ( 'NONE', 3,
 ( #11464, #15014, #6636, #940 ),
 .UNSPECIFIED., .F., .F.,
 ( 4, 4 ),
 ( 0.005123742438166213088, 0.005540500595652342840 ),
 .UNSPECIFIED. ) ;
#13792 = DIRECTION ( 'NONE',  ( -1.000000000000000000, 0.000000000000000000, 0.000000000000000000 ) ) ;
#13793 = ORIENTED_EDGE ( 'NONE', *, *, #9236, .F. ) ;
#13794 = DIRECTION ( 'NONE',  ( 0.000000000000000000, 0.000000000000000000, 1.000000000000000000 ) ) ;
#13795 = CARTESIAN_POINT ( 'NONE',  ( 2.257825467309738876, -26.83036154824992536, -3.467596033028569114 ) ) ;
#13796 = VERTEX_POINT ( 'NONE', #270 ) ;
#13797 = AXIS2_PLACEMENT_3D ( 'NONE', #4449, #3061, #11501 ) ;
#13798 = ORIENTED_EDGE ( 'NONE', *, *, #8887, .F. ) ;
#13799 = EDGE_CURVE ( 'NONE', #4798, #2853, #7793, .T. ) ;
#13800 = SURFACE_STYLE_USAGE ( .BOTH. , #10271 ) ;
#13801 = CYLINDRICAL_SURFACE ( 'NONE', #2406, 13.19999999999999929 ) ;
#13802 = EDGE_CURVE ( 'NONE', #4132, #13815, #9655, .T. ) ;
#13803 = FACE_OUTER_BOUND ( 'NONE', #5098, .T. ) ;
#13804 = CARTESIAN_POINT ( 'NONE',  ( 0.000000000000000000, -20.62201879784905501, -12.52067188844372936 ) ) ;
#13805 = CONTEXT_DEPENDENT_SHAPE_REPRESENTATION ( #11749, #12888 ) ;
#13806 = CARTESIAN_POINT ( 'NONE',  ( 0.000000000000000000, 0.000000000000000000, -2.000000000000000000 ) ) ;
#13807 = ADVANCED_FACE ( 'NONE', ( #5148 ), #349, .F. ) ;
#13808 = CARTESIAN_POINT ( 'NONE',  ( -14.40394475573011945, -10.79473832354794460, -3.794707603699265519E-15 ) ) ;
#13809 = ORIENTED_EDGE ( 'NONE', *, *, #11609, .F. ) ;
#13811 = VECTOR ( 'NONE', #1955, 1000.000000000000000 ) ;
#13810 = FACE_BOUND ( 'NONE', #7494, .T. ) ;
#13812 = DIRECTION ( 'NONE',  ( -1.000000000000000000, 0.000000000000000000, 0.000000000000000000 ) ) ;
#13813 = CARTESIAN_POINT ( 'NONE',  ( 2.790000000000010694, -5.211150952915456713, 13.21889893246973635 ) ) ;
#13814 = EDGE_CURVE ( 'NONE', #6827, #3709, #1166, .T. ) ;
#13815 = VERTEX_POINT ( 'NONE', #8727 ) ;
#13816 = CARTESIAN_POINT ( 'NONE',  ( 2.789999999999999147, 0.000000000000000000, 0.000000000000000000 ) ) ;
#13817 = CARTESIAN_POINT ( 'NONE',  ( 2.604434261026090436, 5.253342437940084153, -25.39738473784996131 ) ) ;
#13818 = EDGE_LOOP ( 'NONE', ( #1599, #10317, #8768, #3678 ) ) ;
#13819 = VERTEX_POINT ( 'NONE', #13420 ) ;
#13820 = CARTESIAN_POINT ( 'NONE',  ( -20.63749999999999574, 0.000000000000000000, 0.000000000000000000 ) ) ;
#13821 = DIRECTION ( 'NONE',  ( -0.000000000000000000, -0.000000000000000000, -1.000000000000000000 ) ) ;
#13822 = ORIENTED_EDGE ( 'NONE', *, *, #9318, .T. ) ;
#13823 = DIRECTION ( 'NONE',  ( 0.000000000000000000, 0.000000000000000000, 1.000000000000000000 ) ) ;
#13824 = LINE ( 'NONE', #14833, #9190 ) ;
#13825 = CARTESIAN_POINT ( 'NONE',  ( 0.000000000000000000, -13.87420763704362869, 1.948757464274129214 ) ) ;
#13826 = CARTESIAN_POINT ( 'NONE',  ( 8.000000000000000000, 0.000000000000000000, 0.000000000000000000 ) ) ;
#13827 = CYLINDRICAL_SURFACE ( 'NONE', #12811, 2.999999999999988898 ) ;
#13828 = ORIENTED_EDGE ( 'NONE', *, *, #309, .T. ) ;
#13829 = PLANE ( 'NONE',  #7530 ) ;
#13830 = CARTESIAN_POINT ( 'NONE',  ( 1.749999999999999778, 17.39253030560841395, 4.458161950358562109 ) ) ;
#13831 = ORIENTED_EDGE ( 'NONE', *, *, #9986, .T. ) ;
#13832 = ORIENTED_EDGE ( 'NONE', *, *, #3197, .F. ) ;
#13833 = ORIENTED_EDGE ( 'NONE', *, *, #2392, .F. ) ;
#13834 = ORIENTED_EDGE ( 'NONE', *, *, #1769, .T. ) ;
#13835 = CARTESIAN_POINT ( 'NONE',  ( 2.789999999999999147, 15.04425356660790136, -20.70663861606255196 ) ) ;
#13836 =( LENGTH_UNIT ( ) NAMED_UNIT ( * ) SI_UNIT ( .MILLI., .METRE. ) );
#13837 = B_SPLINE_CURVE_WITH_KNOTS ( 'NONE', 3,
 ( #315, #14321, #3784, #9860 ),
 .UNSPECIFIED., .F., .F.,
 ( 4, 4 ),
 ( 0.005258110598983608240, 0.005948376585272733066 ),
 .UNSPECIFIED. ) ;
#13838 = CARTESIAN_POINT ( 'NONE',  ( 2.789999999999999147, -24.44424927289185590, 12.96989951879399072 ) ) ;
#13839 = EDGE_CURVE ( 'NONE', #2696, #11370, #14293, .T. ) ;
#13840 = UNCERTAINTY_MEASURE_WITH_UNIT (LENGTH_MEASURE( 1.000000000000000082E-05 ), #6421, 'distance_accuracy_value', 'NONE');
#13842 = CIRCLE ( 'NONE', #1819, 5.575000000000000178 ) ;
#13841 = DIRECTION ( 'NONE',  ( -1.000000000000000000, -0.000000000000000000, -0.000000000000000000 ) ) ;
#13843 = ORIENTED_EDGE ( 'NONE', *, *, #1648, .F. ) ;
#13844 = CIRCLE ( 'NONE', #7951, 28.06981291497571007 ) ;
#13845 = DIRECTION ( 'NONE',  ( 1.000000000000000000, 0.000000000000000000, 0.000000000000000000 ) ) ;
#13846 = DIRECTION ( 'NONE',  ( -1.000000000000000000, -0.000000000000000000, -0.000000000000000000 ) ) ;
#13847 = CARTESIAN_POINT ( 'NONE',  ( 0.2818303507154248932, 15.84037596932093273, -3.072260951847480825 ) ) ;
#13848 = VECTOR ( 'NONE', #8985, 1000.000000000000000 ) ;
#13849 = CIRCLE ( 'NONE', #5027, 31.62277660168379256 ) ;
#13850 = VECTOR ( 'NONE', #4846, 1000.000000000000000 ) ;
#13851 = ORIENTED_EDGE ( 'NONE', *, *, #5247, .T. ) ;
#13852 = DIRECTION ( 'NONE',  ( -1.000000000000000000, -0.000000000000000000, -0.000000000000000000 ) ) ;
#13853 = DIRECTION ( 'NONE',  ( -1.000000000000000000, 0.000000000000000000, 0.000000000000000000 ) ) ;
#13854 = VERTEX_POINT ( 'NONE', #11270 ) ;
#13855 = ORIENTED_EDGE ( 'NONE', *, *, #12420, .T. ) ;
#13856 = CARTESIAN_POINT ( 'NONE',  ( 18.38434835257323030, -21.28306902962084024, 2.000000000000000000 ) ) ;
#13857 = AXIS2_PLACEMENT_3D ( 'NONE', #1902, #8961, #6595 ) ;
#13858 = VECTOR ( 'NONE', #1717, 1000.000000000000227 ) ;
#13859 = EDGE_LOOP ( 'NONE', ( #12552, #2062, #7601, #5890 ) ) ;
#13860 = AXIS2_PLACEMENT_3D ( 'NONE', #6760, #3299, #12664 ) ;
#13861 = ADVANCED_FACE ( 'NONE', ( #744 ), #4438, .F. ) ;
#13862 = CARTESIAN_POINT ( 'NONE',  ( 2.604434404052932805, -19.17825124759790256, 17.45907811351449368 ) ) ;
#13863 = CARTESIAN_POINT ( 'NONE',  ( 0.02436607992776498519, 9.836394144775706394, 22.71065055754456097 ) ) ;
#13864 = CARTESIAN_POINT ( 'NONE',  ( 2.603085161307575834, -14.83319344613228452, 5.279841123861228169 ) ) ;
#13865 = EDGE_LOOP ( 'NONE', ( #10205, #1232, #14253, #6232, #11559, #14330 ) ) ;
#13866 = CARTESIAN_POINT ( 'NONE',  ( 0.000000000000000000, 15.04425356660790136, -20.70663861606255196 ) ) ;
#13867 = DIRECTION ( 'NONE',  ( -1.000000000000000000, -0.000000000000000000, -0.000000000000000000 ) ) ;
#13868 = VERTEX_POINT ( 'NONE', #5445 ) ;
#13869 = AXIS2_PLACEMENT_3D ( 'NONE', #9105, #15024, #8020 ) ;
#13870 = PRODUCT_DEFINITION ( 'UNKNOWN', '', #67, #9786 ) ;
#13871 = EDGE_CURVE ( 'NONE', #14210, #5016, #6811, .T. ) ;
#13872 = CIRCLE ( 'NONE', #1115, 4.999999999999997335 ) ;
#13873 = ADVANCED_FACE ( 'NONE', ( #3046 ), #10192, .T. ) ;
#13874 = AXIS2_PLACEMENT_3D ( 'NONE', #12066, #11836, #4948 ) ;
#13875 = ORIENTED_EDGE ( 'NONE', *, *, #7954, .T. ) ;
#13876 = CYLINDRICAL_SURFACE ( 'NONE', #6333, 0.7500000000000002220 ) ;
#13877 = DIRECTION ( 'NONE',  ( 0.000000000000000000, 0.000000000000000000, 1.000000000000000000 ) ) ;
#13878 = DIRECTION ( 'NONE',  ( 0.000000000000000000, 0.000000000000000000, 1.000000000000000000 ) ) ;
#13879 = CONTEXT_DEPENDENT_SHAPE_REPRESENTATION ( #5680, #11666 ) ;
#13880 = FACE_OUTER_BOUND ( 'NONE', #14897, .T. ) ;
#13881 = PRODUCT_DEFINITION_SHAPE ( 'NONE', 'NONE',  #15240 ) ;
#13882 = CARTESIAN_POINT ( 'NONE',  ( 1.885839517048286229, 4.239993951493212343, 17.20101185194002724 ) ) ;
#13883 = VERTEX_POINT ( 'NONE', #3211 ) ;
#13884 = CARTESIAN_POINT ( 'NONE',  ( -14.40394475573011945, -2.082238426203170629E-15, 16.99999999999999645 ) ) ;
#13885 = LINE ( 'NONE', #7903, #12798 ) ;
#13886 = EDGE_CURVE ( 'NONE', #6954, #3308, #4507, .T. ) ;
#13887 = DIRECTION ( 'NONE',  ( -1.000000000000000000, -0.000000000000000000, 0.000000000000000000 ) ) ;
#13888 = EDGE_CURVE ( 'NONE', #15019, #3945, #4210, .T. ) ;
#13889 = EDGE_LOOP ( 'NONE', ( #5168, #5927, #4854, #7305 ) ) ;
#13890 = EDGE_CURVE ( 'NONE', #14023, #1485, #15166, .T. ) ;
#13891 = CARTESIAN_POINT ( 'NONE',  ( 0.000000000000000000, 2.680914349914567470E-13, -25.59481291497571220 ) ) ;
#13892 = CARTESIAN_POINT ( 'NONE',  ( 1.039999999999997593, 0.000000000000000000, 0.000000000000000000 ) ) ;
#13893 = ORIENTED_EDGE ( 'NONE', *, *, #3471, .F. ) ;
#13894 = EDGE_LOOP ( 'NONE', ( #6753, #13670, #4634, #8166 ) ) ;
#13895 = DIRECTION ( 'NONE',  ( 0.000000000000000000, 0.000000000000000000, 1.000000000000000000 ) ) ;
#13896 = AXIS2_PLACEMENT_3D ( 'NONE', #14528, #6297, #2609 ) ;
#13897 = CARTESIAN_POINT ( 'NONE',  ( 2.262072661820536013, 26.82026385750178932, -3.461047254864356049 ) ) ;
#13898 = ORIENTED_EDGE ( 'NONE', *, *, #14754, .F. ) ;
#13899 = B_SPLINE_CURVE_WITH_KNOTS ( 'NONE', 3,
 ( #5308, #12203, #5230, #362 ),
 .UNSPECIFIED., .F., .F.,
 ( 4, 4 ),
 ( 1.988537749986029444E-07, 0.0006916721208754052263 ),
 .UNSPECIFIED. ) ;
#13900 =( GEOMETRIC_REPRESENTATION_CONTEXT ( 3 ) GLOBAL_UNCERTAINTY_ASSIGNED_CONTEXT ( ( #9925 ) ) GLOBAL_UNIT_ASSIGNED_CONTEXT ( ( #4169, #4005, #1855 ) ) REPRESENTATION_CONTEXT ( 'NONE', 'WORKASPACE' ) );
#13901 = CYLINDRICAL_SURFACE ( 'NONE', #4108, 4.872650870659752442 ) ;
#13902 = DIRECTION ( 'NONE',  ( -1.000000000000000000, -0.000000000000000000, -0.000000000000000000 ) ) ;
#13903 = DIRECTION ( 'NONE',  ( 0.000000000000000000, 0.000000000000000000, 1.000000000000000000 ) ) ;
#13904 = EDGE_CURVE ( 'NONE', #8235, #4803, #12418, .T. ) ;
#13905 = CARTESIAN_POINT ( 'NONE',  ( -5.209999999999999964, 0.000000000000000000, 0.000000000000000000 ) ) ;
#13906 = CARTESIAN_POINT ( 'NONE',  ( 2.789999999999999147, 18.55949924794916228, -16.37294372382838148 ) ) ;
#13907 = ORIENTED_EDGE ( 'NONE', *, *, #11227, .T. ) ;
#13908 = CIRCLE ( 'NONE', #2622, 5.575000000000000178 ) ;
#13909 = CARTESIAN_POINT ( 'NONE',  ( -14.40394475573011945, -10.79473832354794283, -3.000000000000000000 ) ) ;
#13910 = APPLICATION_CONTEXT ( 'automotive_design' ) ;
#13911 = AXIS2_PLACEMENT_3D ( 'NONE', #6481, #13317, #12249 ) ;
#13912 = CARTESIAN_POINT ( 'NONE',  ( 2.789999999999999147, 11.36963888406700285, -9.232963481057645083 ) ) ;
#13913 = ORIENTED_EDGE ( 'NONE', *, *, #9119, .T. ) ;
#13914 = PRESENTATION_LAYER_ASSIGNMENT (  '', '', ( #10716 ) ) ;
#13915 = VECTOR ( 'NONE', #10715, 1000.000000000000000 ) ;
#13916 = PRESENTATION_STYLE_ASSIGNMENT (( #5554 ) ) ;
#13917 = VERTEX_POINT ( 'NONE', #3272 ) ;
#13918 = VERTEX_POINT ( 'NONE', #14884 ) ;
#13919 = ORIENTED_EDGE ( 'NONE', *, *, #9233, .T. ) ;
#13920 = DIRECTION ( 'NONE',  ( -1.000000000000000000, 0.000000000000000000, 0.000000000000000000 ) ) ;
#13921 = AXIS2_PLACEMENT_3D ( 'NONE', #13496, #14431, #417 ) ;
#13922 = CARTESIAN_POINT ( 'NONE',  ( 2.790000000000000036, 0.000000000000000000, 0.000000000000000000 ) ) ;
#13923 = DIRECTION ( 'NONE',  ( -1.000000000000000000, 0.000000000000000000, 0.000000000000000000 ) ) ;
#13924 = CARTESIAN_POINT ( 'NONE',  ( 2.789999999999999147, -21.30679549418640306, 12.59161484032904887 ) ) ;
#13925 = AXIS2_PLACEMENT_3D ( 'NONE', #4280, #12572, #6887 ) ;
#13926 = VERTEX_POINT ( 'NONE', #4278 ) ;
#13927 = CIRCLE ( 'NONE', #3866, 3.799999999999999378 ) ;
#13928 = DIRECTION ( 'NONE',  ( 1.000000000000000000, 0.000000000000000000, 0.000000000000000000 ) ) ;
#13929 = CARTESIAN_POINT ( 'NONE',  ( 19.20634328910001543, -26.21503864878155099, -2.000000000000000000 ) ) ;
#13930 = AXIS2_PLACEMENT_3D ( 'NONE', #7368, #5066, #13266 ) ;
#13931 = VERTEX_POINT ( 'NONE', #15040 ) ;
#13932 = AXIS2_PLACEMENT_3D ( 'NONE', #2500, #7115, #15202 ) ;
#13933 = CARTESIAN_POINT ( 'NONE',  ( 0.7589665349472707323, -4.828387785247840291, -27.14933624560912762 ) ) ;
#13934 = CARTESIAN_POINT ( 'NONE',  ( 2.789999999999999147, -24.04302995059964587, -1.991882183130548878 ) ) ;
#13935 = EDGE_CURVE ( 'NONE', #6223, #516, #889, .T. ) ;
#13936 = AXIS2_PLACEMENT_3D ( 'NONE', #1142, #9360, #11955 ) ;
#13937 = ORIENTED_EDGE ( 'NONE', *, *, #12204, .F. ) ;
#13938 = ORIENTED_EDGE ( 'NONE', *, *, #2059, .F. ) ;
#13939 = TOROIDAL_SURFACE ( 'NONE', #10508, 24.12539914357697413, 8.000000000000000000 ) ;
#13940 = MANIFOLD_SOLID_BREP ( 'Cavity1', #11978 ) ;
#13941 = LINE ( 'NONE', #5879, #1853 ) ;
#13942 = ORIENTED_EDGE ( 'NONE', *, *, #7899, .F. ) ;
#13943 = CARTESIAN_POINT ( 'NONE',  ( 19.25177984293773648, 7.759396820770405157, 3.000000000000002665 ) ) ;
#13944 = CIRCLE ( 'NONE', #12221, 6.000000000000000888 ) ;
#13945 = CARTESIAN_POINT ( 'NONE',  ( 0.000000000000000000, 24.04302995059966364, -1.991882183130399664 ) ) ;
#13946 = EDGE_CURVE ( 'NONE', #5632, #10903, #14186, .T. ) ;
#13947 = CARTESIAN_POINT ( 'NONE',  ( 93.63799900313688340, -2.337932895214617890, 2.999999999999999112 ) ) ;
#13948 = DIRECTION ( 'NONE',  ( -1.000000000000000000, 0.000000000000000000, 0.000000000000000000 ) ) ;
#13949 = VECTOR ( 'NONE', #2347, 1000.000000000000000 ) ;
#13950 = ORIENTED_EDGE ( 'NONE', *, *, #6239, .F. ) ;
#13951 = DIRECTION ( 'NONE',  ( 0.000000000000000000, -1.000000000000000000, -0.000000000000000000 ) ) ;
#13952 = EDGE_CURVE ( 'NONE', #5611, #4786, #8598, .T. ) ;
#13953 = PLANE ( 'NONE',  #9984 ) ;
#13954 = VERTEX_POINT ( 'NONE', #9270 ) ;
#13955 = B_SPLINE_CURVE_WITH_KNOTS ( 'NONE', 3,
 ( #6253, #11090, #7566, #10932, #400, #1417 ),
 .UNSPECIFIED., .F., .F.,
 ( 4, 2, 4 ),
 ( 2.032124546190077199E-07, 0.001878594002992309232, 0.003756984793529999193 ),
 .UNSPECIFIED. ) ;
#13956 = EDGE_CURVE ( 'NONE', #3683, #9176, #6597, .T. ) ;
#13957 = ORIENTED_EDGE ( 'NONE', *, *, #2996, .T. ) ;
#13958 = CARTESIAN_POINT ( 'NONE',  ( -7.718536089453257173E-15, 8.842327429719251342, -11.12243880662604134 ) ) ;
#13959 = CARTESIAN_POINT ( 'NONE',  ( 0.02436607992776325046, -24.15498966839958683, -5.391175441198872598 ) ) ;
#13960 = DIRECTION ( 'NONE',  ( -1.576560579138138762E-17, 1.359337748750801608E-17, -1.000000000000000000 ) ) ;
#13961 = CARTESIAN_POINT ( 'NONE',  ( 2.646101151981377075, 14.59528211759998406, 5.279841123860917307 ) ) ;
#13962 = ITEM_DEFINED_TRANSFORMATION ( 'NONE', 'NONE', #9406,  #1376 ) ;
#13963 = CIRCLE ( 'NONE', #7580, 2.999999999999988898 ) ;
#13964 = DIRECTION ( 'NONE',  ( -0.000000000000000000, -0.000000000000000000, -1.000000000000000000 ) ) ;
#13965 = DIRECTION ( 'NONE',  ( -1.000000000000000000, 0.000000000000000000, 0.000000000000000000 ) ) ;
#13966 = EDGE_CURVE ( 'NONE', #13750, #2791, #8114, .T. ) ;
#13967 = ORIENTED_EDGE ( 'NONE', *, *, #10369, .T. ) ;
#13968 = DIRECTION ( 'NONE',  ( 0.7573544145849105957, -0.6530040510661073716, -2.853163611803960010E-17 ) ) ;
#13969 = ADVANCED_FACE ( 'NONE', ( #10414 ), #15199, .F. ) ;
#13970 = DIRECTION ( 'NONE',  ( 0.000000000000000000, 0.000000000000000000, -1.000000000000000000 ) ) ;
#13971 = CARTESIAN_POINT ( 'NONE',  ( 1.039999999999997815, 17.29145405592688789, 4.835383649608532508 ) ) ;
#13972 = DIRECTION ( 'NONE',  ( -1.000000000000000000, -0.000000000000000000, -0.000000000000000000 ) ) ;
#13973 = ORIENTED_EDGE ( 'NONE', *, *, #14032, .F. ) ;
#13974 = CIRCLE ( 'NONE', #9795, 17.95481323787947403 ) ;
#13975 = DIRECTION ( 'NONE',  ( -0.000000000000000000, -0.000000000000000000, -1.000000000000000000 ) ) ;
#13976 = VERTEX_POINT ( 'NONE', #1042 ) ;
#13977 = EDGE_LOOP ( 'NONE', ( #11182, #12064, #7588, #5812 ) ) ;
#13978 = CARTESIAN_POINT ( 'NONE',  ( 18.40394475573011945, -10.79473832354794460, 5.500000000000000000 ) ) ;
#13979 = LINE ( 'NONE', #3156, #10981 ) ;
#13980 = CARTESIAN_POINT ( 'NONE',  ( 2.765633920072238183, -5.391175441198789109, 24.15498966839961170 ) ) ;
#13981 = DIRECTION ( 'NONE',  ( -0.000000000000000000, -0.000000000000000000, 1.000000000000000000 ) ) ;
#13982 = CARTESIAN_POINT ( 'NONE',  ( 0.02436607992776758727, 24.15498966839963302, 5.391175441198700291 ) ) ;
#13983 = EDGE_CURVE ( 'NONE', #552, #13334, #5671, .T. ) ;
#13984 = CARTESIAN_POINT ( 'NONE',  ( 2.789999999999999147, -14.46287784598619020, 2.311161484776505404 ) ) ;
#13985 = CARTESIAN_POINT ( 'NONE',  ( 0.000000000000000000, 0.4273491293402468805, -0.8000000000000000444 ) ) ;
#13986 = AXIS2_PLACEMENT_3D ( 'NONE', #13826, #14837, #14768 ) ;
#13987 = EDGE_CURVE ( 'NONE', #6372, #132, #1263, .T. ) ;
#13988 = EDGE_CURVE ( 'NONE', #7573, #3010, #11345, .T. ) ;
#13989 = VERTEX_POINT ( 'NONE', #9343 ) ;
#13990 = CARTESIAN_POINT ( 'NONE',  ( 65.21556745095632834, 33.50594455047664866, -2.000000000000000000 ) ) ;
#13991 = CARTESIAN_POINT ( 'NONE',  ( -14.40394475573011590, -4.794738323547945491, 16.99999999999999645 ) ) ;
#13992 = ORIENTED_EDGE ( 'NONE', *, *, #11479, .F. ) ;
#13993 = ORIENTED_EDGE ( 'NONE', *, *, #8095, .T. ) ;
#13994 = ORIENTED_EDGE ( 'NONE', *, *, #11467, .F. ) ;
#13995 = ORIENTED_EDGE ( 'NONE', *, *, #7233, .T. ) ;
#13996 = VECTOR ( 'NONE', #11643, 1000.000000000000000 ) ;
#13997 = FACE_BOUND ( 'NONE', #3823, .T. ) ;
#13998 = CARTESIAN_POINT ( 'NONE',  ( -5.999999999999999112, 0.000000000000000000, 5.500000000000000000 ) ) ;
#13999 = DIRECTION ( 'NONE',  ( 0.000000000000000000, 0.000000000000000000, 1.000000000000000000 ) ) ;
#14000 = CARTESIAN_POINT ( 'NONE',  ( 0.02436607992775891365, -24.63872515616080960, -2.336989772644527008 ) ) ;
#14001 = CARTESIAN_POINT ( 'NONE',  ( 83.50748565343083385, 13.38500995229612478, 2.999999999999999112 ) ) ;
#14002 = EDGE_CURVE ( 'NONE', #6334, #12627, #4769, .T. ) ;
#14003 = ORIENTED_EDGE ( 'NONE', *, *, #13704, .F. ) ;
#14004 = CARTESIAN_POINT ( 'NONE',  ( 0.02436607992775761261, 22.71065055754452544, 9.836394144775786330 ) ) ;
#14005 = EDGE_CURVE ( 'NONE', #13926, #12388, #7112, .T. ) ;
#14006 = ORIENTED_EDGE ( 'NONE', *, *, #13422, .T. ) ;
#14007 = CARTESIAN_POINT ( 'NONE',  ( -1.249999999999997558, 5.633375276077824112E-16, 4.599999999999999645 ) ) ;
#14008 = PRODUCT ( 'short pitch roller chain wheel_s_iso_Chain wheel ISO - 12Z 05B-1 --12SA8.0N', 'short pitch roller chain wheel_s_iso_Chain wheel ISO - 12Z 05B-1 --12SA8.0N', '', ( #1903 ) ) ;
#14009 = CARTESIAN_POINT ( 'NONE',  ( -0.1717365941144614605, -6.008326913195983998, -0.8000000000000000444 ) ) ;
#14010 = ORIENTED_EDGE ( 'NONE', *, *, #13035, .F. ) ;
#14011 = ORIENTED_EDGE ( 'NONE', *, *, #10218, .T. ) ;
#14012 = B_SPLINE_CURVE_WITH_KNOTS ( 'NONE', 3,
 ( #13301, #706, #8771, #13460, #2941, #7700 ),
 .UNSPECIFIED., .F., .F.,
 ( 4, 2, 4 ),
 ( 4.462636793130641501E-07, 0.001879885123570645879, 0.003759323983461978699 ),
 .UNSPECIFIED. ) ;
#14013 = CARTESIAN_POINT ( 'NONE',  ( 0.8291131470075020493, -24.44424927289185590, 12.96989951879399072 ) ) ;
#14014 = ORIENTED_EDGE ( 'NONE', *, *, #5920, .F. ) ;
#14015 = DIRECTION ( 'NONE',  ( -0.000000000000000000, -0.000000000000000000, 1.000000000000000000 ) ) ;
#14016 = CARTESIAN_POINT ( 'NONE',  ( 0.000000000000000000, -1.991882183130148087, -24.04302995059968140 ) ) ;
#14017 = ADVANCED_FACE ( 'NONE', ( #5738 ), #12716, .F. ) ;
#14018 = CARTESIAN_POINT ( 'NONE',  ( 4.271534284832219323E-17, 3.369532131271296443E-15, 6.999999999999989342 ) ) ;
#14019 = DIRECTION ( 'NONE',  ( 0.000000000000000000, 0.000000000000000000, 1.000000000000000000 ) ) ;
#14020 = ORIENTED_EDGE ( 'NONE', *, *, #8625, .T. ) ;
#14021 = DIRECTION ( 'NONE',  ( 1.000000000000000000, 0.000000000000000000, -1.576560579138137530E-17 ) ) ;
#14022 = LINE ( 'NONE', #3564, #5827 ) ;
#14023 = VERTEX_POINT ( 'NONE', #3569 ) ;
#14024 = EDGE_LOOP ( 'NONE', ( #11186, #5921, #10478, #2564 ) ) ;
#14025 = CARTESIAN_POINT ( 'NONE',  ( 1.039999999999998037, -4.835383649608592904, 17.29145405592687368 ) ) ;
#14026 = LINE ( 'NONE', #3494, #11734 ) ;
#14027 = EDGE_CURVE ( 'NONE', #2567, #8808, #13550, .T. ) ;
#14028 = DIRECTION ( 'NONE',  ( 0.000000000000000000, 0.000000000000000000, 1.000000000000000000 ) ) ;
#14029 = FACE_OUTER_BOUND ( 'NONE', #13889, .T. ) ;
#14030 = CONTEXT_DEPENDENT_SHAPE_REPRESENTATION ( #14612, #1371 ) ;
#14031 = CARTESIAN_POINT ( 'NONE',  ( 2.789999999999999147, 4.595504208220027920, 14.19996452731190750 ) ) ;
#14032 = EDGE_CURVE ( 'NONE', #12400, #13089, #6329, .T. ) ;
#14033 = ORIENTED_EDGE ( 'NONE', *, *, #10856, .F. ) ;
#14034 = CARTESIAN_POINT ( 'NONE',  ( -14.40394475573011945, -10.79473832354794460, -3.799999999999999822 ) ) ;
#14035 = DIRECTION ( 'NONE',  ( 1.000000000000000000, 0.000000000000000000, 0.000000000000000000 ) ) ;
#14036 = DIRECTION ( 'NONE',  ( 0.000000000000000000, 0.000000000000000000, 1.000000000000000000 ) ) ;
#14037 = DIRECTION ( 'NONE',  ( 0.000000000000000000, 0.000000000000000000, -1.000000000000000000 ) ) ;
#14038 = AXIS2_PLACEMENT_3D ( 'NONE', #14824, #5527, #1911 ) ;
#14039 = EDGE_LOOP ( 'NONE', ( #15006, #9314, #3923, #1559 ) ) ;
#14040 = EDGE_LOOP ( 'NONE', ( #10646, #3249, #7367, #2636, #2115 ) ) ;
#14041 =( LENGTH_UNIT ( ) NAMED_UNIT ( * ) SI_UNIT ( .MILLI., .METRE. ) );
#14042 = ORIENTED_EDGE ( 'NONE', *, *, #7128, .T. ) ;
#14043 = CARTESIAN_POINT ( 'NONE',  ( -6.082681802200626239E-14, -13.12794558796726641, -5.226347720069425939 ) ) ;
#14044 = CARTESIAN_POINT ( 'NONE',  ( 2.783025325906567371, 2.249040938978837278, -24.42374957165203142 ) ) ;
#14045 = DIRECTION ( 'NONE',  ( -1.000000000000000000, 0.000000000000000000, -0.000000000000000000 ) ) ;
#14046 = CARTESIAN_POINT ( 'NONE',  ( -10.00000000000000000, 0.000000000000000000, 0.000000000000000000 ) ) ;
#14047 = CARTESIAN_POINT ( 'NONE',  ( 2.030753602223783538, 4.828194074574346573, 27.14986936243576565 ) ) ;
#14048 = VECTOR ( 'NONE', #8732, 1000.000000000000000 ) ;
#14049 = CIRCLE ( 'NONE', #2511, 24.12539914357697413 ) ;
#14050 = CARTESIAN_POINT ( 'NONE',  ( 0.000000000000000000, 1.948757464274368578, -13.87420763704359494 ) ) ;
#14051 = DIRECTION ( 'NONE',  ( -0.6310987668242443727, -0.7757024858236036824, -5.947623346206206400E-19 ) ) ;
#14052 = VERTEX_POINT ( 'NONE', #9488 ) ;
#14053 = FACE_OUTER_BOUND ( 'NONE', #10425, .T. ) ;
#14054 = ADVANCED_FACE ( 'NONE', ( #14184, #3648, #8334, #13010, #5204, #3796, #11935 ), #10940, .T. ) ;
#14055 = CARTESIAN_POINT ( 'NONE',  ( 0.006974663525958337516, -12.53640742967767885, 21.08118142846899801 ) ) ;
#14056 = ORIENTED_EDGE ( 'NONE', *, *, #5242, .T. ) ;
#14057 =( NAMED_UNIT ( * ) PLANE_ANGLE_UNIT ( ) SI_UNIT ( $, .RADIAN. ) );
#14058 = VECTOR ( 'NONE', #4959, 1000.000000000000000 ) ;
#14059 = VERTEX_POINT ( 'NONE', #2797 ) ;
#14060 = VERTEX_POINT ( 'NONE', #12088 ) ;
#14061 = VERTEX_POINT ( 'NONE', #250 ) ;
#14062 = CARTESIAN_POINT ( 'NONE',  ( 72.68384697807672978, 11.35494834827056110, 2.999999999999999112 ) ) ;
#14063 = EDGE_CURVE ( 'NONE', #6211, #9636, #530, .T. ) ;
#14064 = CARTESIAN_POINT ( 'NONE',  ( 0.7795480827049480199, -5.008579424861446583, -16.73367785739762326 ) ) ;
#14065 = ADVANCED_FACE ( 'NONE', ( #9868 ), #2568, .F. ) ;
#14066 = EDGE_CURVE ( 'NONE', #15036, #3632, #1914, .T. ) ;
#14067 = PLANE ( 'NONE',  #13698 ) ;
#14068 = CARTESIAN_POINT ( 'NONE',  ( 69.97572749000833880, 15.55805301486455683, 4.000000000000000000 ) ) ;
#14069 = B_SPLINE_CURVE_WITH_KNOTS ( 'NONE', 3,
 ( #8669, #373, #13362, #2842, #688, #11063, #14764, #4231 ),
 .UNSPECIFIED., .F., .F.,
 ( 4, 2, 2, 4 ),
 ( 2.154797737779156328E-07, 0.001895231411415139412, 0.002842739377235820215, 0.003790247343056500802 ),
 .UNSPECIFIED. ) ;
#14070 = LINE ( 'NONE', #2394, #11519 ) ;
#14071 = ORIENTED_EDGE ( 'NONE', *, *, #10788, .T. ) ;
#14072 = CARTESIAN_POINT ( 'NONE',  ( 67.45386469005195806, 13.93318132202354676, 2.999999999999999112 ) ) ;
#14073 = EDGE_CURVE ( 'NONE', #14197, #7731, #14416, .T. ) ;
#14074 = EDGE_CURVE ( 'NONE', #3861, #13918, #7333, .T. ) ;
#14075 = VERTEX_POINT ( 'NONE', #6339 ) ;
#14076 = FACE_OUTER_BOUND ( 'NONE', #6993, .T. ) ;
#14077 = DIRECTION ( 'NONE',  ( -0.9237280213470681067, -0.3830490080632377725, 0.000000000000000000 ) ) ;
#14078 = ADVANCED_FACE ( 'NONE', ( #7422 ), #2879, .F. ) ;
#14079 = ORIENTED_EDGE ( 'NONE', *, *, #3826, .F. ) ;
#14080 = ORIENTED_EDGE ( 'NONE', *, *, #9236, .T. ) ;
#14081 = CIRCLE ( 'NONE', #11138, 4.100000000000000533 ) ;
#14082 = B_SPLINE_CURVE_WITH_KNOTS ( 'NONE', 3,
 ( #1835, #13283, #1612, #14373 ),
 .UNSPECIFIED., .F., .F.,
 ( 4, 4 ),
 ( 3.059063720795852959E-07, 0.0006888942284914018055 ),
 .UNSPECIFIED. ) ;
#14083 = CARTESIAN_POINT ( 'NONE',  ( 0.02531912748631468327, -14.46287784598615644, -2.311161484776706576 ) ) ;
#14084 = EDGE_CURVE ( 'NONE', #12769, #12877, #3961, .T. ) ;
#14085 = VERTEX_POINT ( 'NONE', #7351 ) ;
#14086 = DIRECTION ( 'NONE',  ( 1.000000000000000000, 0.000000000000000000, 0.000000000000000000 ) ) ;
#14087 = B_SPLINE_CURVE_WITH_KNOTS ( 'NONE', 3,
 ( #9791, #8467, #14488, #6020 ),
 .UNSPECIFIED., .F., .F.,
 ( 4, 4 ),
 ( 0.005258105385878687407, 0.005948373736081388405 ),
 .UNSPECIFIED. ) ;
#14088 = CARTESIAN_POINT ( 'NONE',  ( 2.262072706628479146, -19.66369668717046437, 18.56460150496932116 ) ) ;
#14089 = AXIS2_PLACEMENT_3D ( 'NONE', #7327, #3546, #10698 ) ;
#14090 = DIRECTION ( 'NONE',  ( 0.000000000000000000, 0.000000000000000000, 1.000000000000000000 ) ) ;
#14091 = CARTESIAN_POINT ( 'NONE',  ( 80.00000000000000000, -9.999999999999994671, 4.000000000000003553 ) ) ;
#14092 = VECTOR ( 'NONE', #13448, 999.9999999999998863 ) ;
#14093 = ORIENTED_EDGE ( 'NONE', *, *, #14618, .T. ) ;
#14094 = B_SPLINE_CURVE_WITH_KNOTS ( 'NONE', 3,
 ( #9319, #6486, #12606, #1010, #12684, #935, #3246, #4554 ),
 .UNSPECIFIED., .F., .F.,
 ( 4, 2, 2, 4 ),
 ( 4.663089342001531929E-07, 0.001898630032275743168, 0.002847711893946511599, 0.003796793755617280681 ),
 .UNSPECIFIED. ) ;
#14095 = CYLINDRICAL_SURFACE ( 'NONE', #4858, 6.000000000000000000 ) ;
#14096 = LINE ( 'NONE', #1112, #13915 ) ;
#14097 = ORIENTED_EDGE ( 'NONE', *, *, #6466, .T. ) ;
#14098 = ORIENTED_EDGE ( 'NONE', *, *, #8893, .T. ) ;
#14099 = DIRECTION ( 'NONE',  ( -1.000000000000000000, 0.000000000000000000, 0.000000000000000000 ) ) ;
#14101 = CARTESIAN_POINT ( 'NONE',  ( 2.789999999999999147, -12.59161484032927092, 21.30679549418627161 ) ) ;
#14100 = VECTOR ( 'NONE', #3448, 1000.000000000000000 ) ;
#14102 = CIRCLE ( 'NONE', #6747, 3.799999999999999378 ) ;
#14103 = VECTOR ( 'NONE', #1726, 1000.000000000000000 ) ;
#14104 = CARTESIAN_POINT ( 'NONE',  ( 2.764680872515352661, 5.229914364928351489, 13.68080036884350292 ) ) ;
#14105 = CARTESIAN_POINT ( 'NONE',  ( 0.02436607992775934733, -21.30679549418640306, 12.59161484032904887 ) ) ;
#14106 = CARTESIAN_POINT ( 'NONE',  ( -15.94493884710238696, -7.321218896460230496, -3.000000000000000000 ) ) ;
#14107 = CARTESIAN_POINT ( 'NONE',  ( 0.000000000000000000, -18.28042085475288303, 15.74360496233377305 ) ) ;
#14108 = ORIENTED_EDGE ( 'NONE', *, *, #5813, .T. ) ;
#14109 = LINE ( 'NONE', #8123, #14202 ) ;
#14110 = DIRECTION ( 'NONE',  ( 1.000000000000000000, 0.000000000000000000, 0.000000000000000000 ) ) ;
#14111 = MANIFOLD_SOLID_BREP ( 'Notch', #11131 ) ;
#14112 = PRODUCT_DEFINITION_FORMATION_WITH_SPECIFIED_SOURCE ( 'ANY', '', #11046, .NOT_KNOWN. ) ;
#14113 = DIRECTION ( 'NONE',  ( 1.000000000000000000, 0.000000000000000000, 0.000000000000000000 ) ) ;
#14114 = AXIS2_PLACEMENT_3D ( 'NONE', #8339, #11856, #10642 ) ;
#14115 = DIRECTION ( 'NONE',  ( 0.000000000000000000, 0.000000000000000000, 1.000000000000000000 ) ) ;
#14116 = ORIENTED_EDGE ( 'NONE', *, *, #6724, .F. ) ;
#14117 = AXIS2_PLACEMENT_3D ( 'NONE', #2253, #3330, #8015 ) ;
#14118 = ORIENTED_EDGE ( 'NONE', *, *, #8052, .T. ) ;
#14119 = CARTESIAN_POINT ( 'NONE',  ( 60.61028236725008611, -31.15713940066886067, 4.000000000000000000 ) ) ;
#14120 = ORIENTED_EDGE ( 'NONE', *, *, #5790, .T. ) ;
#14121 = CARTESIAN_POINT ( 'NONE',  ( 2.789999999999999147, 0.000000000000000000, 0.000000000000000000 ) ) ;
#14122 = CARTESIAN_POINT ( 'NONE',  ( 0.006974657972265168107, -5.408388659524262287, 23.92335783895635970 ) ) ;
#14123 = DIRECTION ( 'NONE',  ( 0.4571871344001385284, 0.8893705212896308998, 0.000000000000000000 ) ) ;
#14124 = CARTESIAN_POINT ( 'NONE',  ( 0.02531912748606228100, -13.68080036884352246, 5.229914364928304416 ) ) ;
#14125 = DIRECTION ( 'NONE',  ( 0.9975010064204040683, -0.07065226245691946794, 0.000000000000000000 ) ) ;
#14126 = CARTESIAN_POINT ( 'NONE',  ( 2.601776091974069338, 5.251266773802368171, 25.40949241676355541 ) ) ;
#14127 = AXIS2_PLACEMENT_3D ( 'NONE', #9871, #10031, #6414 ) ;
#14128 = ORIENTED_EDGE ( 'NONE', *, *, #2429, .T. ) ;
#14129 = CARTESIAN_POINT ( 'NONE',  ( -9.999999999999998224, -1.390791565672605534, -131.1575142076926852 ) ) ;
#14130 = DIRECTION ( 'NONE',  ( 0.000000000000000000, 0.000000000000000000, 1.000000000000000000 ) ) ;
#14131 = ORIENTED_EDGE ( 'NONE', *, *, #13799, .T. ) ;
#14132 = DIRECTION ( 'NONE',  ( 0.000000000000000000, 0.000000000000000000, 1.000000000000000000 ) ) ;
#14133 = FACE_OUTER_BOUND ( 'NONE', #6231, .T. ) ;
#14134 =( NAMED_UNIT ( * ) PLANE_ANGLE_UNIT ( ) SI_UNIT ( $, .RADIAN. ) );
#14135 = ORIENTED_EDGE ( 'NONE', *, *, #876, .T. ) ;
#14136 = VECTOR ( 'NONE', #14760, 1000.000000000000000 ) ;
#14137 = EDGE_CURVE ( 'NONE', #1390, #6218, #4869, .T. ) ;
#14138 =( NAMED_UNIT ( * ) SI_UNIT ( $, .STERADIAN. ) SOLID_ANGLE_UNIT ( ) );
#14139 = EDGE_LOOP ( 'NONE', ( #12015, #10213, #276, #1909 ) ) ;
#14140 = ORIENTED_EDGE ( 'NONE', *, *, #10030, .F. ) ;
#14141 = VERTEX_POINT ( 'NONE', #7496 ) ;
#14142 = LINE ( 'NONE', #9531, #3854 ) ;
#14143 = DIRECTION ( 'NONE',  ( -1.000000000000000000, 0.000000000000000000, 0.000000000000000000 ) ) ;
#14144 = EDGE_CURVE ( 'NONE', #11100, #12913, #6040, .T. ) ;
#14145 = DIRECTION ( 'NONE',  ( -1.000000000000000000, 0.000000000000000000, -0.000000000000000000 ) ) ;
#14146 = CARTESIAN_POINT ( 'NONE',  ( 2.508169649284527569, -3.072260951847640698, 15.84037596932107483 ) ) ;
#14147 = VECTOR ( 'NONE', #11967, 1000.000000000000000 ) ;
#14148 = CARTESIAN_POINT ( 'NONE',  ( 0.1920563539683088072, -2.883512197589118475, 15.58455734132165560 ) ) ;
#14149 = CIRCLE ( 'NONE', #2125, 28.06981291497571007 ) ;
#14150 = EDGE_LOOP ( 'NONE', ( #6113, #13469, #1461, #8679 ) ) ;
#14151 = CARTESIAN_POINT ( 'NONE',  ( 111.6227766016837961, 7.610970684806392799E-15, 7.000000000000000000 ) ) ;
#14152 = COLOUR_RGB ( '',0.8941176470588234615, 0.8941176470588234615, 0.8941176470588234615 ) ;
#14153 = AXIS2_PLACEMENT_3D ( 'NONE', #4733, #8111, #9561 ) ;
#14154 = EDGE_CURVE ( 'NONE', #12618, #11359, #12165, .T. ) ;
#14155 = ADVANCED_FACE ( 'NONE', ( #2086 ), #5782, .T. ) ;
#14156 = AXIS2_PLACEMENT_3D ( 'NONE', #10514, #5967, #8192 ) ;
#14157 = AXIS2_PLACEMENT_3D ( 'NONE', #462, #1850, #14387 ) ;
#14158 = ORIENTED_EDGE ( 'NONE', *, *, #7880, .T. ) ;
#14159 = CARTESIAN_POINT ( 'NONE',  ( 1.749999999999998002, 12.52377138324259143, -25.12109765559640451 ) ) ;
#14160 = DIRECTION ( 'NONE',  ( 0.000000000000000000, 0.000000000000000000, 1.000000000000000000 ) ) ;
#14161 = VERTEX_POINT ( 'NONE', #5561 ) ;
#14162 = ORIENTED_EDGE ( 'NONE', *, *, #1857, .T. ) ;
#14163 = TOROIDAL_SURFACE ( 'NONE', #10961, 24.12539914357697413, 8.000000000000000000 ) ;
#14164 = AXIS2_PLACEMENT_3D ( 'NONE', #13268, #665, #4140 ) ;
#14165 = DIRECTION ( 'NONE',  ( 0.1643989873053574580, -0.9863939238321436376, 0.000000000000000000 ) ) ;
#14166 = ADVANCED_FACE ( 'NONE', ( #12321, #11457 ), #9234, .F. ) ;
#14167 = ORIENTED_EDGE ( 'NONE', *, *, #574, .F. ) ;
#14168 = CIRCLE ( 'NONE', #13434, 28.06981291497571362 ) ;
#14169 = LINE ( 'NONE', #2719, #9435 ) ;
#14170 = DIRECTION ( 'NONE',  ( 0.000000000000000000, 0.000000000000000000, -1.000000000000000000 ) ) ;
#14171 = EDGE_CURVE ( 'NONE', #10675, #8188, #14094, .T. ) ;
#14172 = CARTESIAN_POINT ( 'NONE',  ( 0.02436607992776498519, 9.836394144775706394, 22.71065055754456097 ) ) ;
#14173 = CARTESIAN_POINT ( 'NONE',  ( 2.789999999999999147, 24.44424927289185945, 12.96989951879416125 ) ) ;
#14174 = CIRCLE ( 'NONE', #3615, 4.000000000000000888 ) ;
#14175 = ORIENTED_EDGE ( 'NONE', *, *, #14545, .T. ) ;
#14176 = COLOUR_RGB ( '',0.8941176470588234615, 0.8941176470588234615, 0.8941176470588234615 ) ;
#14177 = DIRECTION ( 'NONE',  ( -1.000000000000000000, -0.000000000000000000, -0.000000000000000000 ) ) ;
#14178 = CARTESIAN_POINT ( 'NONE',  ( 2.764680872515354881, -13.68080036884352246, 5.229914364928304416 ) ) ;
#14179 = AXIS2_PLACEMENT_3D ( 'NONE', #5295, #1746, #13339 ) ;
#14180 = CIRCLE ( 'NONE', #9512, 4.000000000000000000 ) ;
#14181 = ORIENTED_EDGE ( 'NONE', *, *, #10568, .F. ) ;
#14182 = EDGE_CURVE ( 'NONE', #7470, #13819, #2402, .T. ) ;
#14183 = ORIENTED_EDGE ( 'NONE', *, *, #1543, .F. ) ;
#14184 = FACE_BOUND ( 'NONE', #8525, .T. ) ;
#14185 = LINE ( 'NONE', #11711, #11005 ) ;
#14186 = CIRCLE ( 'NONE', #15175, 24.12539914357697413 ) ;
#14187 = CARTESIAN_POINT ( 'NONE',  ( 2.740003281797978474, 5.264737421541524576, 13.99876742897260939 ) ) ;
#14188 = CARTESIAN_POINT ( 'NONE',  ( 19.25177984293775424, 7.759396820770413150, 7.000000000000006217 ) ) ;
#14189 = CARTESIAN_POINT ( 'NONE',  ( 0.0003207540509378258692, 20.70663861606293921, -12.51925356660738053 ) ) ;
#14190 = VECTOR ( 'NONE', #7294, 1000.000000000000000 ) ;
#14191 = DIRECTION ( 'NONE',  ( 1.000000000000000000, 0.000000000000000000, 0.000000000000000000 ) ) ;
#14192 = ORIENTED_EDGE ( 'NONE', *, *, #932, .F. ) ;
#14193 = CARTESIAN_POINT ( 'NONE',  ( 1.749999999999998002, 20.02152543075346003, 19.67366047555537634 ) ) ;
#14194 = CARTESIAN_POINT ( 'NONE',  ( 1.150000000000001688, 0.000000000000000000, 0.000000000000000000 ) ) ;
#14195 = CARTESIAN_POINT ( 'NONE',  ( 1.394999999999999574, -24.89775460606823287, -12.96210679857813908 ) ) ;
#14196 = DIRECTION ( 'NONE',  ( -1.000000000000000000, -0.000000000000000000, -0.000000000000000000 ) ) ;
#14197 = VERTEX_POINT ( 'NONE', #8086 ) ;
#14198 = ORIENTED_EDGE ( 'NONE', *, *, #11681, .T. ) ;
#14199 = ADVANCED_FACE ( 'NONE', ( #4477 ), #11533, .F. ) ;
#14200 = EDGE_LOOP ( 'NONE', ( #13101, #894 ) ) ;
#14201 = CIRCLE ( 'NONE', #9293, 4.872650870659752442 ) ;
#14202 = VECTOR ( 'NONE', #12725, 1000.000000000000000 ) ;
#14203 = CARTESIAN_POINT ( 'NONE',  ( 19.20634328910001543, -26.21503864878155099, 5.000000000000000000 ) ) ;
#14204 = DIRECTION ( 'NONE',  ( 0.9728364810787193395, 0.2314933715733012431, 0.000000000000000000 ) ) ;
#14205 = DIRECTION ( 'NONE',  ( 0.8893705212896308998, -0.4571871344001385284, 0.000000000000000000 ) ) ;
#14206 = DIRECTION ( 'NONE',  ( 1.445602896647338917E-16, -1.000000000000000000, 0.000000000000000000 ) ) ;
#14207 = DIRECTION ( 'NONE',  ( 0.000000000000000000, 0.000000000000000000, -1.000000000000000000 ) ) ;
#14208 = CARTESIAN_POINT ( 'NONE',  ( 8.000000000000000000, 0.000000000000000000, 0.000000000000000000 ) ) ;
#14209 = B_SPLINE_CURVE_WITH_KNOTS ( 'NONE', 3,
 ( #4637, #2699, #11900, #5011, #13130, #3530 ),
 .UNSPECIFIED., .F., .F.,
 ( 4, 2, 4 ),
 ( 2.586195665699493951E-07, 0.001878649493629688805, 0.003757040367692807744 ),
 .UNSPECIFIED. ) ;
#14210 = VERTEX_POINT ( 'NONE', #2243 ) ;
#14211 = CARTESIAN_POINT ( 'NONE',  ( 0.02531912748631555063, 2.311161484776756758, -14.46287784598614756 ) ) ;
#14212 = CARTESIAN_POINT ( 'NONE',  ( -9.999999999999992895, -25.00000000000000000, 6.000000000000000000 ) ) ;
#14213 = ORIENTED_EDGE ( 'NONE', *, *, #901, .F. ) ;
#14214 = EDGE_CURVE ( 'NONE', #11373, #12711, #5119, .T. ) ;
#14215 = CARTESIAN_POINT ( 'NONE',  ( 0.000000000000000000, -20.70663861606260170, -15.04425356660783031 ) ) ;
#14216 = CARTESIAN_POINT ( 'NONE',  ( 0.006931038682727856497, -12.53626894672812853, -21.08061549536629187 ) ) ;
#14217 = AXIS2_PLACEMENT_3D ( 'NONE', #8406, #1344, #1657 ) ;
#14218 = AXIS2_PLACEMENT_3D ( 'NONE', #6815, #7039, #3574 ) ;
#14219 = PRESENTATION_STYLE_ASSIGNMENT (( #9524 ) ) ;
#14220 = EDGE_CURVE ( 'NONE', #10087, #10003, #10616, .T. ) ;
#14221 = ORIENTED_EDGE ( 'NONE', *, *, #1254, .F. ) ;
#14222 = ORIENTED_EDGE ( 'NONE', *, *, #8580, .F. ) ;
#14223 = ORIENTED_EDGE ( 'NONE', *, *, #6823, .F. ) ;
#14224 = ORIENTED_EDGE ( 'NONE', *, *, #146, .T. ) ;
#14225 = PLANE ( 'NONE',  #4349 ) ;
#14226 = CARTESIAN_POINT ( 'NONE',  ( 1.394999999999999574, 27.68468304288259318, 4.633866840649019103 ) ) ;
#14227 = CARTESIAN_POINT ( 'NONE',  ( 1.039999999999999369, -12.52377138324206918, -25.12109765559666741 ) ) ;
#14228 = CARTESIAN_POINT ( 'NONE',  ( 2.337784053193427525, -11.13074453164194644, -12.42068120944093046 ) ) ;
#14229 = CIRCLE ( 'NONE', #2939, 28.06981291497571362 ) ;
#14230 = EDGE_CURVE ( 'NONE', #4505, #13954, #7131, .T. ) ;
#14231 = CARTESIAN_POINT ( 'NONE',  ( 2.765633920072234631, 16.37294372382885044, -18.55949924794875017 ) ) ;
#14232 = B_SPLINE_CURVE_WITH_KNOTS ( 'NONE', 3,
 ( #14290, #208, #4928, #9597, #3751, #1152, #8432, #13119 ),
 .UNSPECIFIED., .F., .F.,
 ( 4, 2, 2, 4 ),
 ( 2.445728210282408609E-07, 0.001895260649874690694, 0.002842768688401522276, 0.003790276726928353424 ),
 .UNSPECIFIED. ) ;
#14233 = EDGE_CURVE ( 'NONE', #5968, #11548, #14646, .T. ) ;
#14234 = VERTEX_POINT ( 'NONE', #10381 ) ;
#14235 = DIRECTION ( 'NONE',  ( 1.000000000000000000, 0.000000000000000000, 0.000000000000000000 ) ) ;
#14236 = VECTOR ( 'NONE', #121, 1000.000000000000000 ) ;
#14237 = ORIENTED_EDGE ( 'NONE', *, *, #6101, .T. ) ;
#14238 = PLANE ( 'NONE',  #3567 ) ;
#14239 = CARTESIAN_POINT ( 'NONE',  ( 2.257825491203654611, 24.44564404695844573, 11.58891744060115947 ) ) ;
#14240 = ORIENTED_EDGE ( 'NONE', *, *, #7289, .F. ) ;
#14241 = ORIENTED_EDGE ( 'NONE', *, *, #5081, .F. ) ;
#14242 = EDGE_CURVE ( 'NONE', #10147, #9857, #934, .T. ) ;
#14243 = CARTESIAN_POINT ( 'NONE',  ( -0.1374368770859597522, -4.808326913195983821, -0.8000000000000000444 ) ) ;
#14244 = VERTEX_POINT ( 'NONE', #12827 ) ;
#14245 = DIRECTION ( 'NONE',  ( -1.445602896647338917E-16, 1.000000000000000000, 0.000000000000000000 ) ) ;
#14246 = DIRECTION ( 'NONE',  ( -1.000000000000000000, -0.000000000000000000, -0.000000000000000000 ) ) ;
#14247 = CARTESIAN_POINT ( 'NONE',  ( 0.1085714285714285687, -3.798448662927795372, -0.8000000000000000444 ) ) ;
#14248 = DIRECTION ( 'NONE',  ( 0.000000000000000000, 0.000000000000000000, 1.000000000000000000 ) ) ;
#14249 = EDGE_CURVE ( 'NONE', #14052, #3287, #4627, .T. ) ;
#14250 = ORIENTED_EDGE ( 'NONE', *, *, #1570, .F. ) ;
#14251 = CARTESIAN_POINT ( 'NONE',  ( 2.789999999999999147, 0.000000000000000000, 0.000000000000000000 ) ) ;
#14252 = CARTESIAN_POINT ( 'NONE',  ( 2.790000000000061320, -13.21862218141519563, 5.211197193340646017 ) ) ;
#14253 = ORIENTED_EDGE ( 'NONE', *, *, #14847, .F. ) ;
#14254 = CARTESIAN_POINT ( 'NONE',  ( 4.747884751462026820, -5.143694235355983579, 0.000000000000000000 ) ) ;
#14255 = VERTEX_POINT ( 'NONE', #10237 ) ;
#14256 = ORIENTED_EDGE ( 'NONE', *, *, #6381, .F. ) ;
#14257 = DIRECTION ( 'NONE',  ( 0.000000000000000000, 0.000000000000000000, 1.000000000000000000 ) ) ;
#14258 = DIRECTION ( 'NONE',  ( -1.000000000000000000, 0.000000000000000000, -0.000000000000000000 ) ) ;
#14259 = EDGE_CURVE ( 'NONE', #4276, #3346, #3147, .T. ) ;
#14260 = ADVANCED_FACE ( 'NONE', ( #11760, #8445 ), #14067, .T. ) ;
#14261 = DIRECTION ( 'NONE',  ( 0.000000000000000000, 0.000000000000000000, 1.000000000000000000 ) ) ;
#14262 = DIRECTION ( 'NONE',  ( -0.000000000000000000, -0.000000000000000000, 1.000000000000000000 ) ) ;
#14263 = SHAPE_REPRESENTATION ( 'short pitch roller chain wheel_s_iso_Chain wheel ISO - 20Z 05B-1 --20SA8.0N', ( #1376 ), #11929 ) ;
#14264 = CARTESIAN_POINT ( 'NONE',  ( 111.6227766016837961, 7.610970684806392799E-15, -131.1575142076926852 ) ) ;
#14265 = CARTESIAN_POINT ( 'NONE',  ( 2.789999999999999147, -1.948757464274269102, 13.87420763704360560 ) ) ;
#14266 = ORIENTED_EDGE ( 'NONE', *, *, #3814, .T. ) ;
#14267 = CARTESIAN_POINT ( 'NONE',  ( -1.250000000000001110, 6.827405905246494173E-16, 5.575000000000000178 ) ) ;
#14268 = CARTESIAN_POINT ( 'NONE',  ( 2.789999999999999147, -8.624777288397876163, 11.04103753892268713 ) ) ;
#14269 = DIRECTION ( 'NONE',  ( -1.000000000000000000, 0.000000000000000000, 0.000000000000000000 ) ) ;
#14270 = CARTESIAN_POINT ( 'NONE',  ( 0.0001048950922011769414, -20.67847077765692632, -12.51925356660783351 ) ) ;
#14271 = ORIENTED_EDGE ( 'NONE', *, *, #9777, .T. ) ;
#14272 = EDGE_CURVE ( 'NONE', #12669, #12714, #8223, .T. ) ;
#14273 = VERTEX_POINT ( 'NONE', #5862 ) ;
#14274 = EDGE_CURVE ( 'NONE', #1566, #1423, #6077, .T. ) ;
#14275 = ORIENTED_EDGE ( 'NONE', *, *, #3097, .T. ) ;
#14276 = CARTESIAN_POINT ( 'NONE',  ( 0.7686372158811272115, 11.98841295390598027, 12.71987259277439719 ) ) ;
#14277 = CARTESIAN_POINT ( 'NONE',  ( 2.789999999999999147, 11.04103753892271556, 8.624777288397840636 ) ) ;
#14278 = ADVANCED_FACE ( 'NONE', ( #2390 ), #7324, .T. ) ;
#14279 = DIRECTION ( 'NONE',  ( 1.000000000000000000, 0.000000000000000000, 0.000000000000000000 ) ) ;
#14280 = CARTESIAN_POINT ( 'NONE',  ( 2.789999999999999147, -15.04425356660744839, -20.70663861606288236 ) ) ;
#14281 = DIRECTION ( 'NONE',  ( -0.9336186042270442353, -0.3582684773199361628, -0.000000000000000000 ) ) ;
#14282 = CARTESIAN_POINT ( 'NONE',  ( 62.65957446808508280, 26.91300136313512681, -8.169391093593850073 ) ) ;
#14283 = ORIENTED_EDGE ( 'NONE', *, *, #13679, .F. ) ;
#14284 = DIRECTION ( 'NONE',  ( 1.000000000000000000, 0.000000000000000000, 0.000000000000000000 ) ) ;
#14285 = CYLINDRICAL_SURFACE ( 'NONE', #3056, 2.524999999999998579 ) ;
#14286 = ADVANCED_FACE ( 'NONE', ( #6152 ), #1238, .T. ) ;
#14287 = VERTEX_POINT ( 'NONE', #7394 ) ;
#14288 = CARTESIAN_POINT ( 'NONE',  ( 0.000000000000000000, 0.000000000000000000, 4.000000000000000000 ) ) ;
#14289 = VECTOR ( 'NONE', #413, 1000.000000000000000 ) ;
#14290 = CARTESIAN_POINT ( 'NONE',  ( 0.02531912748679390063, 9.232963481057920418, -11.36963888406677725 ) ) ;
#14291 = CARTESIAN_POINT ( 'NONE',  ( 0.000000000000000000, -12.52067188844364587, 20.62201879784910119 ) ) ;
#14292 = ORIENTED_EDGE ( 'NONE', *, *, #5553, .F. ) ;
#14293 = B_SPLINE_CURVE_WITH_KNOTS ( 'NONE', 3,
 ( #2901, #6426, #11340, #965, #10115, #11490 ),
 .UNSPECIFIED., .F., .F.,
 ( 4, 2, 4 ),
 ( 2.132675795051084930E-07, 0.001878604073277006722, 0.003756994878974508241 ),
 .UNSPECIFIED. ) ;
#14294 = ORIENTED_EDGE ( 'NONE', *, *, #2192, .F. ) ;
#14295 = EDGE_LOOP ( 'NONE', ( #10958, #6922 ) ) ;
#14296 = ORIENTED_EDGE ( 'NONE', *, *, #9336, .T. ) ;
#14297 = DIRECTION ( 'NONE',  ( 1.000000000000000000, 0.000000000000000000, 0.000000000000000000 ) ) ;
#14298 = CARTESIAN_POINT ( 'NONE',  ( -9.403944755730117677, -16.79473832354794993, 12.00000000000000000 ) ) ;
#14299 = VECTOR ( 'NONE', #8423, 1000.000000000000000 ) ;
#14300 = AXIS2_PLACEMENT_3D ( 'NONE', #12411, #6581, #3124 ) ;
#14301 = CARTESIAN_POINT ( 'NONE',  ( 0.4522159373304741048, 16.32199768300079157, 3.429166897524482227 ) ) ;
#14302 = CARTESIAN_POINT ( 'NONE',  ( -2.141980652367355020, -6.189445006155633422, -0.8000000000000000444 ) ) ;
#14303 = DIRECTION ( 'NONE',  ( 0.7573544145849105957, -0.6530040510661073716, -2.081668171172162967E-17 ) ) ;
#14304 = CARTESIAN_POINT ( 'NONE',  ( 0.2076373213219097902, -2.899259574942639972, -15.57879356040266217 ) ) ;
#14305 = EDGE_LOOP ( 'NONE', ( #6147, #9294, #6504, #3594 ) ) ;
#14306 = CARTESIAN_POINT ( 'NONE',  ( 0.000000000000000000, -20.62201879784923264, 12.52067188844344336 ) ) ;
#14307 = EDGE_CURVE ( 'NONE', #6387, #12769, #3622, .T. ) ;
#14308 = AXIS2_PLACEMENT_3D ( 'NONE', #11927, #14560, #8628 ) ;
#14309 = B_SPLINE_CURVE_WITH_KNOTS ( 'NONE', 3,
 ( #5747, #3362, #9416, #10733, #7195, #3505 ),
 .UNSPECIFIED., .F., .F.,
 ( 4, 2, 4 ),
 ( 4.462636793131339774E-07, 0.001879885123570645012, 0.003759323983461976965 ),
 .UNSPECIFIED. ) ;
#14310 = B_SPLINE_CURVE_WITH_KNOTS ( 'NONE', 3,
 ( #4861, #12983, #11980, #1386 ),
 .UNSPECIFIED., .F., .F.,
 ( 4, 4 ),
 ( 0.005258110598983628189, 0.005948376585272736536 ),
 .UNSPECIFIED. ) ;
#14311 = ORIENTED_EDGE ( 'NONE', *, *, #9192, .F. ) ;
#14312 = FACE_OUTER_BOUND ( 'NONE', #10860, .T. ) ;
#14313 = EDGE_CURVE ( 'NONE', #3242, #3993, #13944, .T. ) ;
#14314 = LINE ( 'NONE', #12912, #2093 ) ;
#14315 = ORIENTED_EDGE ( 'NONE', *, *, #7407, .T. ) ;
#14316 = ORIENTED_EDGE ( 'NONE', *, *, #37, .T. ) ;
#14317 = DIRECTION ( 'NONE',  ( -0.000000000000000000, -0.000000000000000000, 1.000000000000000000 ) ) ;
#14318 = ORIENTED_EDGE ( 'NONE', *, *, #8964, .F. ) ;
#14319 = CARTESIAN_POINT ( 'NONE',  ( 2.789999999999999147, -23.48180575137726223, -5.535312321042966666 ) ) ;
#14320 = CARTESIAN_POINT ( 'NONE',  ( 0.07186813532171169860, -2.577209017047189299, 25.22589920183361301 ) ) ;
#14321 = CARTESIAN_POINT ( 'NONE',  ( 2.790000000000000480, 15.96500990068124715, 18.34424029220116736 ) ) ;
#14322 = DIRECTION ( 'NONE',  ( 0.000000000000000000, 0.000000000000000000, -1.000000000000000000 ) ) ;
#14323 = VERTEX_POINT ( 'NONE', #5996 ) ;
#14324 = LINE ( 'NONE', #243, #6944 ) ;
#14325 = FACE_OUTER_BOUND ( 'NONE', #4031, .T. ) ;
#14326 = ORIENTED_EDGE ( 'NONE', *, *, #12634, .T. ) ;
#14327 = CARTESIAN_POINT ( 'NONE',  ( 0.5537796877189847811, 12.52687487503418851, 11.41743294611079484 ) ) ;
#14328 = EDGE_CURVE ( 'NONE', #10057, #6030, #10266, .T. ) ;
#14329 = VERTEX_POINT ( 'NONE', #60 ) ;
#14330 = ORIENTED_EDGE ( 'NONE', *, *, #8292, .F. ) ;
#14331 = SURFACE_STYLE_USAGE ( .BOTH. , #4965 ) ;
#14332 = FACE_OUTER_BOUND ( 'NONE', #10255, .T. ) ;
#14333 = CARTESIAN_POINT ( 'NONE',  ( 1.039999999999996261, 12.96210679857786197, 24.89775460606836788 ) ) ;
#14334 = EDGE_CURVE ( 'NONE', #3966, #5767, #691, .T. ) ;
#14335 = CONTEXT_DEPENDENT_SHAPE_REPRESENTATION ( #9386, #3328 ) ;
#14336 = CARTESIAN_POINT ( 'NONE',  ( 0.02531912748631078014, -2.311161484776655950, 14.46287784598616355 ) ) ;
#14337 = VECTOR ( 'NONE', #8854, 1000.000000000000000 ) ;
#14338 = CARTESIAN_POINT ( 'NONE',  ( 0.000000000000000000, 0.000000000000000000, 0.000000000000000000 ) ) ;
#14339 = CIRCLE ( 'NONE', #12370, 9.999999999999994671 ) ;
#14340 = ORIENTED_EDGE ( 'NONE', *, *, #170, .F. ) ;
#14341 = FACE_OUTER_BOUND ( 'NONE', #12855, .T. ) ;
#14342 = TOROIDAL_SURFACE ( 'NONE', #9914, 24.12539914357697768, 8.000000000000000000 ) ;
#14343 = CARTESIAN_POINT ( 'NONE',  ( -20.63749999999999929, 0.000000000000000000, -4.599999999999999645 ) ) ;
#14344 = CARTESIAN_POINT ( 'NONE',  ( 2.789999999999999147, 0.000000000000000000, 0.000000000000000000 ) ) ;
#14345 = CARTESIAN_POINT ( 'NONE',  ( 83.50748565343083385, 13.38500995229612478, 6.000000000000000000 ) ) ;
#14346 = ADVANCED_FACE ( 'NONE', ( #4780 ), #9451, .F. ) ;
#14347 = ADVANCED_FACE ( 'NONE', ( #3613 ), #4938, .T. ) ;
#14348 = ORIENTED_EDGE ( 'NONE', *, *, #4035, .F. ) ;
#14349 = ORIENTED_EDGE ( 'NONE', *, *, #13585, .T. ) ;
#14350 = AXIS2_PLACEMENT_3D ( 'NONE', #10745, #7286, #2369 ) ;
#14351 = AXIS2_PLACEMENT_3D ( 'NONE', #5469, #9991, #13757 ) ;
#14352 = ORIENTED_EDGE ( 'NONE', *, *, #2621, .T. ) ;
#14353 = VECTOR ( 'NONE', #12283, 1000.000000000000000 ) ;
#14354 = DIRECTION ( 'NONE',  ( -0.9863939238321437486, -0.1643989873053572359, 0.000000000000000000 ) ) ;
#14355 = CARTESIAN_POINT ( 'NONE',  ( 0.07186808533286707934, 10.24630254990548650, -23.19485392143201707 ) ) ;
#14356 = CARTESIAN_POINT ( 'NONE',  ( -16.80212006966224791, -13.74240776967763900, 0.7999999999999960476 ) ) ;
#14357 = FACE_OUTER_BOUND ( 'NONE', #11230, .T. ) ;
#14358 = CARTESIAN_POINT ( 'NONE',  ( 14.40394475573011945, -10.79473832354794460, -7.800000000000006928 ) ) ;
#14359 = FACE_OUTER_BOUND ( 'NONE', #6310, .T. ) ;
#14360 = VERTEX_POINT ( 'NONE', #7154 ) ;
#14361 = CARTESIAN_POINT ( 'NONE',  ( 1.039999999999996705, -20.02152543075331081, -19.67366047555552555 ) ) ;
#14362 = CARTESIAN_POINT ( 'NONE',  ( 1.039999999999999369, -12.52377138324206918, -25.12109765559666741 ) ) ;
#14363 = AXIS2_PLACEMENT_3D ( 'NONE', #14046, #8281, #5915 ) ;
#14364 = EDGE_CURVE ( 'NONE', #11164, #2043, #304, .T. ) ;
#14365 = CIRCLE ( 'NONE', #12132, 14.01039946648074341 ) ;
#14366 = VERTEX_POINT ( 'NONE', #14227 ) ;
#14367 = CARTESIAN_POINT ( 'NONE',  ( 80.00000000000000000, 0.000000000000000000, 6.000000000000000000 ) ) ;
#14368 = CARTESIAN_POINT ( 'NONE',  ( 2.765633920072242624, 9.836394144775706394, 22.71065055754456097 ) ) ;
#14369 = CARTESIAN_POINT ( 'NONE',  ( -14.40394475573011945, -10.79473832354794283, -3.000000000000000000 ) ) ;
#14370 = EDGE_CURVE ( 'NONE', #132, #3713, #7675, .T. ) ;
#14371 = ORIENTED_EDGE ( 'NONE', *, *, #7864, .T. ) ;
#14372 = CARTESIAN_POINT ( 'NONE',  ( 2.697960371751379149, -9.756102650610319671, 11.73065272960059602 ) ) ;
#14373 = CARTESIAN_POINT ( 'NONE',  ( 0.000000000000000000, 22.25075486061751207, -9.324097380959241121 ) ) ;
#14374 = ORIENTED_EDGE ( 'NONE', *, *, #7049, .T. ) ;
#14375 = VERTEX_POINT ( 'NONE', #13222 ) ;
#14376 = ORIENTED_EDGE ( 'NONE', *, *, #3663, .F. ) ;
#14377 = DIRECTION ( 'NONE',  ( 0.000000000000000000, 0.000000000000000000, 1.000000000000000000 ) ) ;
#14378 = DIRECTION ( 'NONE',  ( 5.480158469902919838E-17, 1.051478716308701618E-16, 1.000000000000000000 ) ) ;
#14379 = EDGE_CURVE ( 'NONE', #7299, #8724, #9044, .T. ) ;
#14380 = VECTOR ( 'NONE', #5253, 1000.000000000000000 ) ;
#14381 = VECTOR ( 'NONE', #4200, 1000.000000000000000 ) ;
#14382 = DIRECTION ( 'NONE',  ( -1.000000000000000000, -0.000000000000000000, -0.000000000000000000 ) ) ;
#14383 = CARTESIAN_POINT ( 'NONE',  ( 3.510166481118872639, 1.455586230640303791, -7.800000000000008704 ) ) ;
#14384 = CARTESIAN_POINT ( 'NONE',  ( 0.000000000000000000, -1.948757464274081030, -13.87420763704363580 ) ) ;
#14385 = CARTESIAN_POINT ( 'NONE',  ( 1.749999999999998002, 20.02152543075374069, -19.67366047555509212 ) ) ;
#14386 = EDGE_LOOP ( 'NONE', ( #762, #590, #8920, #8061, #12095, #2923 ) ) ;
#14387 = DIRECTION ( 'NONE',  ( 0.000000000000000000, 0.000000000000000000, 1.000000000000000000 ) ) ;
#14388 = AXIS2_PLACEMENT_3D ( 'NONE', #5030, #9620, #5191 ) ;
#14389 = B_SPLINE_CURVE_WITH_KNOTS ( 'NONE', 3,
 ( #10937, #12399, #4028, #11021 ),
 .UNSPECIFIED., .F., .F.,
 ( 4, 4 ),
 ( 0.005258110598983589158, 0.005948376585272731332 ),
 .UNSPECIFIED. ) ;
#14390 =( NAMED_UNIT ( * ) SI_UNIT ( $, .STERADIAN. ) SOLID_ANGLE_UNIT ( ) );
#14391 = ORIENTED_EDGE ( 'NONE', *, *, #5699, .T. ) ;
#14392 = VERTEX_POINT ( 'NONE', #6379 ) ;
#14393 = CARTESIAN_POINT ( 'NONE',  ( 4.747884751462026820, -5.143694235355983579, -0.8000000000000000444 ) ) ;
#14394 = PRODUCT ( 'spacer', 'spacer', '', ( #4057 ) ) ;
#14395 = CYLINDRICAL_SURFACE ( 'NONE', #8455, 0.7500000000000002220 ) ;
#14396 = AXIS2_PLACEMENT_3D ( 'NONE', #4238, #8914, #12454 ) ;
#14397 = EDGE_LOOP ( 'NONE', ( #13833, #10456, #4291, #10035 ) ) ;
#14398 = VECTOR ( 'NONE', #827, 1000.000000000000000 ) ;
#14399 = LINE ( 'NONE', #3867, #3577 ) ;
#14400 = ORIENTED_EDGE ( 'NONE', *, *, #6970, .F. ) ;
#14401 = CARTESIAN_POINT ( 'NONE',  ( 0.0003207540509378258692, 20.70663861606293921, -12.51925356660738053 ) ) ;
#14402 = CARTESIAN_POINT ( 'NONE',  ( -5.209999999999999964, 0.000000000000000000, 0.000000000000000000 ) ) ;
#14403 = CARTESIAN_POINT ( 'NONE',  ( 1.250000000000001110, 0.000000000000000000, -5.400000000000000355 ) ) ;
#14404 = VECTOR ( 'NONE', #14659, 1000.000000000000000 ) ;
#14405 = VECTOR ( 'NONE', #224, 1000.000000000000000 ) ;
#14406 = ORIENTED_EDGE ( 'NONE', *, *, #13060, .T. ) ;
#14407 = CARTESIAN_POINT ( 'NONE',  ( 101.6227766016837819, 5.204170427930421283E-15, 4.000000000000003553 ) ) ;
#14408 = EDGE_CURVE ( 'NONE', #495, #14244, #14811, .T. ) ;
#14409 = FACE_OUTER_BOUND ( 'NONE', #8666, .T. ) ;
#14410 = VECTOR ( 'NONE', #370, 1000.000000000000000 ) ;
#14411 = ORIENTED_EDGE ( 'NONE', *, *, #13027, .F. ) ;
#14412 = CARTESIAN_POINT ( 'NONE',  ( -16.92833982302709828, -13.89754826684236022, -5.000000000000000000 ) ) ;
#14413 = CARTESIAN_POINT ( 'NONE',  ( 0.02531912748606228100, -13.68080036884352246, 5.229914364928304416 ) ) ;
#14414 = VERTEX_POINT ( 'NONE', #9904 ) ;
#14415 = ORIENTED_EDGE ( 'NONE', *, *, #1277, .F. ) ;
#14416 = LINE ( 'NONE', #14568, #14693 ) ;
#14417 = DIRECTION ( 'NONE',  ( -0.000000000000000000, -0.000000000000000000, -1.000000000000000000 ) ) ;
#14418 = AXIS2_PLACEMENT_3D ( 'NONE', #13866, #6499, #4664 ) ;
#14419 = FACE_BOUND ( 'NONE', #1532, .T. ) ;
#14420 = ADVANCED_FACE ( 'NONE', ( #5239 ), #5319, .T. ) ;
#14421 = B_SPLINE_CURVE_WITH_KNOTS ( 'NONE', 3,
 ( #7791, #14863, #866, #14948, #4257, #14787, #3253, #10091 ),
 .UNSPECIFIED., .F., .F.,
 ( 4, 2, 2, 4 ),
 ( 2.032124546156068561E-07, 0.001631739532304432192, 0.002447507692229335726, 0.003263275852154239043 ),
 .UNSPECIFIED. ) ;
#14422 = AXIS2_PLACEMENT_3D ( 'NONE', #8131, #8199, #2290 ) ;
#14423 = DIRECTION ( 'NONE',  ( 1.000000000000000000, 0.000000000000000000, -2.710505431213761085E-17 ) ) ;
#14424 = AXIS2_PLACEMENT_3D ( 'NONE', #5068, #3906, #12034 ) ;
#14425 = EDGE_CURVE ( 'NONE', #4113, #11392, #8947, .T. ) ;
#14426 = ORIENTED_EDGE ( 'NONE', *, *, #8508, .F. ) ;
#14427 = CARTESIAN_POINT ( 'NONE',  ( -9.999999999999998224, 0.000000000000000000, -130.1575142076926852 ) ) ;
#14428 = CARTESIAN_POINT ( 'NONE',  ( -1.000000000000000222, -4.808326913195983821, -0.8000000000000000444 ) ) ;
#14429 = AXIS2_PLACEMENT_3D ( 'NONE', #3294, #13821, #4459 ) ;
#14430 = DIRECTION ( 'NONE',  ( 0.000000000000000000, 0.9510565162951567508, -0.3090169943749379589 ) ) ;
#14431 = DIRECTION ( 'NONE',  ( 0.000000000000000000, 0.000000000000000000, 1.000000000000000000 ) ) ;
#14432 = ORIENTED_EDGE ( 'NONE', *, *, #779, .F. ) ;
#14433 = EDGE_CURVE ( 'NONE', #2534, #13239, #3930, .T. ) ;
#14434 = ADVANCED_BREP_SHAPE_REPRESENTATION ( '', ( #13393, #1376 ), #2887 ) ;
#14435 = ORIENTED_EDGE ( 'NONE', *, *, #8691, .F. ) ;
#14436 = VERTEX_POINT ( 'NONE', #3074 ) ;
#14437 = AXIS2_PLACEMENT_3D ( 'NONE', #11677, #13999, #3399 ) ;
#14438 = AXIS2_PLACEMENT_3D ( 'NONE', #3723, #11715, #9274 ) ;
#14439 = CARTESIAN_POINT ( 'NONE',  ( 1.039999999999996927, 12.55714665600005375, -12.83329210556818545 ) ) ;
#14440 = DIRECTION ( 'NONE',  ( 0.000000000000000000, 0.000000000000000000, -1.000000000000000000 ) ) ;
#14441 = CARTESIAN_POINT ( 'NONE',  ( 1.749999999999998002, -4.147968289691086774, -27.76164181293056288 ) ) ;
#14442 = CYLINDRICAL_SURFACE ( 'NONE', #1100, 13.19999999999999929 ) ;
#14443 = CARTESIAN_POINT ( 'NONE',  ( 0.000000000000000000, 0.000000000000000000, -5.290000000000000924 ) ) ;
#14444 = LINE ( 'NONE', #14282, #14299 ) ;
#14445 = EDGE_CURVE ( 'NONE', #14273, #12521, #3161, .T. ) ;
#14446 = VERTEX_POINT ( 'NONE', #7759 ) ;
#14447 = DIRECTION ( 'NONE',  ( 1.576560579138138762E-17, -1.359337748750801608E-17, 1.000000000000000000 ) ) ;
#14448 = CARTESIAN_POINT ( 'NONE',  ( -4.000000000000000888, 0.000000000000000000, -7.800000000000010481 ) ) ;
#14449 = ORIENTED_EDGE ( 'NONE', *, *, #4677, .F. ) ;
#14450 = CARTESIAN_POINT ( 'NONE',  ( 14.40394475573011945, -10.79473832354794460, 6.000000000000000000 ) ) ;
#14451 = CARTESIAN_POINT ( 'NONE',  ( 2.789999999999999591, 2.133490293297010343, 24.22479935914660132 ) ) ;
#14452 = AXIS2_PLACEMENT_3D ( 'NONE', #15142, #9216, #14915 ) ;
#14453 = CARTESIAN_POINT ( 'NONE',  ( 2.765633920072234631, -21.30679549418640306, 12.59161484032904887 ) ) ;
#14454 = ORIENTED_EDGE ( 'NONE', *, *, #7016, .F. ) ;
#14455 = EDGE_CURVE ( 'NONE', #14511, #10310, #1608, .T. ) ;
#14456 = AXIS2_PLACEMENT_3D ( 'NONE', #14068, #1084, #3400 ) ;
#14457 = CARTESIAN_POINT ( 'NONE',  ( 54.00962148274519592, 34.79915921274093193, 4.000000000000000000 ) ) ;
#14458 = CARTESIAN_POINT ( 'NONE',  ( 0.09203966225861301420, -15.03709480088673445, 2.583706482361980861 ) ) ;
#14459 = ORIENTED_EDGE ( 'NONE', *, *, #12009, .T. ) ;
#14460 = ORIENTED_EDGE ( 'NONE', *, *, #11990, .F. ) ;
#14461 = VERTEX_POINT ( 'NONE', #5399 ) ;
#14462 = DIRECTION ( 'NONE',  ( 0.000000000000000000, 0.000000000000000000, 1.000000000000000000 ) ) ;
#14463 = EDGE_CURVE ( 'NONE', #4099, #5041, #10998, .T. ) ;
#14464 = CARTESIAN_POINT ( 'NONE',  ( 0.000000000000000000, -11.04103753892265871, -8.624777288397922348 ) ) ;
#14465 = DIRECTION ( 'NONE',  ( -1.000000000000000000, -0.000000000000000000, 0.000000000000000000 ) ) ;
#14466 = DIRECTION ( 'NONE',  ( -1.000000000000000000, -0.000000000000000000, -0.000000000000000000 ) ) ;
#14467 = CARTESIAN_POINT ( 'NONE',  ( -14.40394475573011945, -10.79473832354794460, 0.7999999999999960476 ) ) ;
#14468 = EDGE_CURVE ( 'NONE', #1007, #1420, #2334, .T. ) ;
#14469 = EDGE_CURVE ( 'NONE', #3403, #6654, #10421, .T. ) ;
#14470 = CARTESIAN_POINT ( 'NONE',  ( 0.000000000000000000, 5.249430348645754307, 12.98979500319696534 ) ) ;
#14471 = CIRCLE ( 'NONE', #2190, 6.000000000000005329 ) ;
#14472 = CIRCLE ( 'NONE', #7059, 4.000000000000000888 ) ;
#14473 = VECTOR ( 'NONE', #9642, 1000.000000000000000 ) ;
#14474 = ORIENTED_EDGE ( 'NONE', *, *, #6198, .F. ) ;
#14475 = CARTESIAN_POINT ( 'NONE',  ( 0.006930995026448713570, 5.408431875071442185, 23.92277630352796791 ) ) ;
#14476 = EDGE_LOOP ( 'NONE', ( #4773, #12302 ) ) ;
#14477 = VERTEX_POINT ( 'NONE', #5174 ) ;
#14478 = EDGE_CURVE ( 'NONE', #2037, #40, #1928, .T. ) ;
#14479 = CIRCLE ( 'NONE', #6630, 20.00000000000000000 ) ;
#14480 = CARTESIAN_POINT ( 'NONE',  ( 0.000000000000000000, 8.624777288397805108, 11.04103753892274575 ) ) ;
#14481 = EDGE_CURVE ( 'NONE', #11965, #5795, #12217, .T. ) ;
#14482 = CARTESIAN_POINT ( 'NONE',  ( 1.394999999999998685, -17.39253030560838198, -4.458161950358684678 ) ) ;
#14483 = ORIENTED_EDGE ( 'NONE', *, *, #8037, .T. ) ;
#14484 = EDGE_CURVE ( 'NONE', #11577, #1894, #14069, .T. ) ;
#14485 = DIRECTION ( 'NONE',  ( -1.000000000000000000, 5.782411586589353694E-16, 0.000000000000000000 ) ) ;
#14486 = ORIENTED_EDGE ( 'NONE', *, *, #12246, .F. ) ;
#14487 = DIRECTION ( 'NONE',  ( -0.9237280213470681067, -0.3830490080632377725, 0.000000000000000000 ) ) ;
#14488 = CARTESIAN_POINT ( 'NONE',  ( 2.783068888626319293, -22.53293026234510776, 9.685942809246967045 ) ) ;
#14489 = AXIS2_PLACEMENT_3D ( 'NONE', #14673, #4215, #7741 ) ;
#14490 = ADVANCED_FACE ( 'NONE', ( #7541 ), #523, .T. ) ;
#14491 = CARTESIAN_POINT ( 'NONE',  ( 0.7592463965288815952, 12.98165646470117274, -24.32906614999601302 ) ) ;
#14492 = DIRECTION ( 'NONE',  ( -0.000000000000000000, -0.000000000000000000, -1.000000000000000000 ) ) ;
#14493 = CARTESIAN_POINT ( 'NONE',  ( 0.04999670013151429060, 11.55877992729678638, -9.490919315500011777 ) ) ;
#14494 = ORIENTED_EDGE ( 'NONE', *, *, #5583, .F. ) ;
#14495 = DIRECTION ( 'NONE',  ( -1.000000000000000000, 0.000000000000000000, 0.000000000000000000 ) ) ;
#14496 = CARTESIAN_POINT ( 'NONE',  ( 2.597943565934061283, -14.93837896275546306, -5.295083827234870810 ) ) ;
#14497 = ORIENTED_EDGE ( 'NONE', *, *, #4012, .F. ) ;
#14498 = ORIENTED_EDGE ( 'NONE', *, *, #13026, .F. ) ;
#14499 = FILL_AREA_STYLE_COLOUR ( '', #10503 ) ;
#14500 = AXIS2_PLACEMENT_3D ( 'NONE', #8425, #5074, #2685 ) ;
#14501 = CARTESIAN_POINT ( 'NONE',  ( 0.4472135954999577612, 6.613092715395707467E-16, -5.400000000000000355 ) ) ;
#14502 = DIRECTION ( 'NONE',  ( 0.000000000000000000, 0.000000000000000000, 1.000000000000000000 ) ) ;
#14503 = DIRECTION ( 'NONE',  ( -0.000000000000000000, -0.000000000000000000, 1.000000000000000000 ) ) ;
#14504 = DIRECTION ( 'NONE',  ( -0.000000000000000000, -0.000000000000000000, 1.000000000000000000 ) ) ;
#14505 = ORIENTED_EDGE ( 'NONE', *, *, #15010, .F. ) ;
#14506 = DIRECTION ( 'NONE',  ( 0.000000000000000000, 0.000000000000000000, 1.000000000000000000 ) ) ;
#14507 = CYLINDRICAL_SURFACE ( 'NONE', #9870, 2.524999999999999467 ) ;
#14508 = DIRECTION ( 'NONE',  ( 0.000000000000000000, 0.000000000000000000, 1.000000000000000000 ) ) ;
#14509 = DIRECTION ( 'NONE',  ( -1.000000000000000000, -0.000000000000000000, -0.000000000000000000 ) ) ;
#14510 = ORIENTED_EDGE ( 'NONE', *, *, #12567, .T. ) ;
#14511 = VERTEX_POINT ( 'NONE', #3297 ) ;
#14512 = ORIENTED_EDGE ( 'NONE', *, *, #10826, .F. ) ;
#14513 = CARTESIAN_POINT ( 'NONE',  ( 15.21482963846748504, 16.90833299098317610, 4.000000000000003553 ) ) ;
#14514 = DIRECTION ( 'NONE',  ( 1.000000000000000000, 0.000000000000000000, 0.000000000000000000 ) ) ;
#14515 = ADVANCED_FACE ( 'NONE', ( #12525 ), #3158, .T. ) ;
#14516 = DIRECTION ( 'NONE',  ( 1.000000000000000000, 0.000000000000000000, 0.000000000000000000 ) ) ;
#14517 = LINE ( 'NONE', #8654, #3077 ) ;
#14518 = APPLICATION_PROTOCOL_DEFINITION ( 'draft international standard', 'automotive_design', 1998, #8310 ) ;
#14519 = CYLINDRICAL_SURFACE ( 'NONE', #11833, 4.000000000000000000 ) ;
#14520 = ORIENTED_EDGE ( 'NONE', *, *, #10696, .F. ) ;
#14521 = CARTESIAN_POINT ( 'NONE',  ( 0.5279272933715204452, -19.66369668717018726, -18.56460150496961248 ) ) ;
#14522 = DIRECTION ( 'NONE',  ( -0.000000000000000000, -0.000000000000000000, -1.000000000000000000 ) ) ;
#14523 = ORIENTED_EDGE ( 'NONE', *, *, #2661, .T. ) ;
#14524 = FACE_OUTER_BOUND ( 'NONE', #651, .T. ) ;
#14525 = CYLINDRICAL_SURFACE ( 'NONE', #387, 3.000000000000000888 ) ;
#14526 = LINE ( 'NONE', #5163, #1589 ) ;
#14527 = ORIENTED_EDGE ( 'NONE', *, *, #4388, .T. ) ;
#14528 = CARTESIAN_POINT ( 'NONE',  ( 1.749999999999998002, 0.000000000000000000, 0.000000000000000000 ) ) ;
#14529 = CARTESIAN_POINT ( 'NONE',  ( 1.039999999999997149, -17.39253030560844948, 4.458161950358441317 ) ) ;
#14530 = VERTEX_POINT ( 'NONE', #4385 ) ;
#14531 = ORIENTED_EDGE ( 'NONE', *, *, #520, .T. ) ;
#14532 = DIRECTION ( 'NONE',  ( -1.000000000000000000, -0.000000000000000000, -0.000000000000000000 ) ) ;
#14533 = DIRECTION ( 'NONE',  ( 1.445602896647338917E-16, -1.000000000000000000, 0.000000000000000000 ) ) ;
#14534 = CARTESIAN_POINT ( 'NONE',  ( 1.149999999999998135, 0.000000000000000000, 0.000000000000000000 ) ) ;
#14535 = CARTESIAN_POINT ( 'NONE',  ( 1.394999999999999574, -4.835383649608353984, -17.29145405592693763 ) ) ;
#14536 = CARTESIAN_POINT ( 'NONE',  ( 0.02531912748464761401, -2.311161484776455222, -14.46287784598619908 ) ) ;
#14537 = EDGE_CURVE ( 'NONE', #5734, #1566, #13706, .T. ) ;
#14538 = CARTESIAN_POINT ( 'NONE',  ( 80.00000000000000000, 0.000000000000000000, 5.500000000000005329 ) ) ;
#14539 = ORIENTED_EDGE ( 'NONE', *, *, #4622, .F. ) ;
#14540 = B_SPLINE_CURVE_WITH_KNOTS ( 'NONE', 3,
 ( #14004, #5644, #6703, #10318, #11383, #4559 ),
 .UNSPECIFIED., .F., .F.,
 ( 4, 2, 4 ),
 ( 2.586195665686417350E-07, 0.001878649493629684251, 0.003757040367692799938 ),
 .UNSPECIFIED. ) ;
#14541 = DIRECTION ( 'NONE',  ( 0.000000000000000000, 0.000000000000000000, 1.000000000000000000 ) ) ;
#14542 = PRODUCT_RELATED_PRODUCT_CATEGORY ( 'part', '', ( #11046 ) ) ;
#14543 = EDGE_CURVE ( 'NONE', #3632, #1378, #13207, .T. ) ;
#14544 = AXIS2_PLACEMENT_3D ( 'NONE', #5746, #15128, #4601 ) ;
#14545 = EDGE_CURVE ( 'NONE', #1997, #14980, #10517, .T. ) ;
#14546 = EDGE_LOOP ( 'NONE', ( #4724, #3192, #4171, #15140 ) ) ;
#14547 = ORIENTED_EDGE ( 'NONE', *, *, #6101, .F. ) ;
#14548 = ORIENTED_EDGE ( 'NONE', *, *, #14455, .T. ) ;
#14549 = CARTESIAN_POINT ( 'NONE',  ( 0.000000000000000000, -7.909232158574647009, -21.81711360614308148 ) ) ;
#14550 = CARTESIAN_POINT ( 'NONE',  ( 93.63799900313689761, -2.337932895214617002, 7.000000000000000000 ) ) ;
#14551 = ORIENTED_EDGE ( 'NONE', *, *, #309, .F. ) ;
#14552 = UNCERTAINTY_MEASURE_WITH_UNIT (LENGTH_MEASURE( 1.000000000000000082E-05 ), #10078, 'distance_accuracy_value', 'NONE');
#14553 = FACE_OUTER_BOUND ( 'NONE', #11279, .T. ) ;
#14554 = EDGE_LOOP ( 'NONE', ( #14296, #2447, #6907, #12336, #9915, #8236, #4062, #8494 ) ) ;
#14555 = CARTESIAN_POINT ( 'NONE',  ( 93.63799900313688340, -2.337932895214617890, 7.000000000000000000 ) ) ;
#14556 = FACE_OUTER_BOUND ( 'NONE', #14883, .T. ) ;
#14557 = EDGE_CURVE ( 'NONE', #5808, #9595, #4001, .T. ) ;
#14558 = EDGE_CURVE ( 'NONE', #3287, #14052, #5861, .T. ) ;
#14559 = CARTESIAN_POINT ( 'NONE',  ( -1.566204647097437563, -6.822536405429463713, 0.000000000000000000 ) ) ;
#14560 = DIRECTION ( 'NONE',  ( -1.000000000000000000, 0.000000000000000000, -0.000000000000000000 ) ) ;
#14561 = EDGE_CURVE ( 'NONE', #5438, #13461, #1056, .T. ) ;
#14562 = CARTESIAN_POINT ( 'NONE',  ( 1.039999999999998037, 12.83329210556849276, -12.55714665599973756 ) ) ;
#14563 = VERTEX_POINT ( 'NONE', #2067 ) ;
#14564 = CARTESIAN_POINT ( 'NONE',  ( 0.1920564340659368097, 14.93837896275556609, -5.295083827234559060 ) ) ;
#14565 = CYLINDRICAL_SURFACE ( 'NONE', #13367, 8.400000000000000355 ) ;
#14566 = ORIENTED_EDGE ( 'NONE', *, *, #6391, .F. ) ;
#14567 = ORIENTED_EDGE ( 'NONE', *, *, #511, .F. ) ;
#14568 = CARTESIAN_POINT ( 'NONE',  ( 1.394999999999999574, -12.55714665599996138, 12.83329210556827249 ) ) ;
#14569 = DIRECTION ( 'NONE',  ( 0.000000000000000000, 0.000000000000000000, -1.000000000000000000 ) ) ;
#14570 = EDGE_CURVE ( 'NONE', #14980, #14624, #8519, .T. ) ;
#14571 = FILL_AREA_STYLE_COLOUR ( '', #6577 ) ;
#14572 = DIRECTION ( 'NONE',  ( 1.000000000000000000, 0.000000000000000000, 0.000000000000000000 ) ) ;
#14573 = DIRECTION ( 'NONE',  ( 1.000000000000000000, -0.000000000000000000, -0.000000000000000000 ) ) ;
#14574 = ORIENTED_EDGE ( 'NONE', *, *, #9458, .F. ) ;
#14575 = DIRECTION ( 'NONE',  ( -0.9863939238321436376, -0.1643989873053573192, 0.000000000000000000 ) ) ;
#14576 = CARTESIAN_POINT ( 'NONE',  ( 1.666666666666673624, 0.000000000000000000, 7.000000000000000000 ) ) ;
#14577 = DIRECTION ( 'NONE',  ( -1.000000000000000000, 0.000000000000000000, 0.000000000000000000 ) ) ;
#14578 = CARTESIAN_POINT ( 'NONE',  ( 54.00962148274520302, 34.79915921274093193, 6.000000000000000000 ) ) ;
#14579 = ORIENTED_EDGE ( 'NONE', *, *, #11356, .F. ) ;
#14580 = ORIENTED_EDGE ( 'NONE', *, *, #13512, .F. ) ;
#14581 = ORIENTED_EDGE ( 'NONE', *, *, #376, .F. ) ;
#14582 = CARTESIAN_POINT ( 'NONE',  ( 0.07181525480391401373, -21.92234060054336098, -12.74223776959224708 ) ) ;
#14583 = FACE_OUTER_BOUND ( 'NONE', #3941, .T. ) ;
#14584 = CARTESIAN_POINT ( 'NONE',  ( 2.718184767880468922, -23.19431517146925970, -10.24584646439563507 ) ) ;
#14585 = CARTESIAN_POINT ( 'NONE',  ( 2.765633920072235963, -5.391175441198450713, -24.15498966839968276 ) ) ;
#14586 = APPLICATION_PROTOCOL_DEFINITION ( 'draft international standard', 'automotive_design', 1998, #13013 ) ;
#14587 = CARTESIAN_POINT ( 'NONE',  ( 2.337784068222783951, 5.191253194756234812, -15.84984805378626049 ) ) ;
#14588 = AXIS2_PLACEMENT_3D ( 'NONE', #5802, #2332, #3141 ) ;
#14589 = DIRECTION ( 'NONE',  ( -1.000000000000000000, -0.000000000000000000, -0.000000000000000000 ) ) ;
#14590 = CARTESIAN_POINT ( 'NONE',  ( 0.1882238552569854284, -10.68696068830390900, -23.64332819722392287 ) ) ;
#14591 = ORIENTED_EDGE ( 'NONE', *, *, #9566, .T. ) ;
#14592 = CARTESIAN_POINT ( 'NONE',  ( 1.749999999999999778, -4.458161950358378256, -17.39253030560846369 ) ) ;
#14593 = LINE ( 'NONE', #12282, #5805 ) ;
#14594 = CARTESIAN_POINT ( 'NONE',  ( -5.209999999999999964, 0.000000000000000000, 0.000000000000000000 ) ) ;
#14595 = EDGE_LOOP ( 'NONE', ( #8365, #10154, #7306, #9833, #2280, #2478 ) ) ;
#14596 = CIRCLE ( 'NONE', #7960, 3.799999999999998934 ) ;
#14597 = AXIS2_PLACEMENT_3D ( 'NONE', #14845, #15067, #9149 ) ;
#14598 = EDGE_CURVE ( 'NONE', #4547, #8287, #498, .T. ) ;
#14599 = CARTESIAN_POINT ( 'NONE',  ( 75.20570977803312473, 12.97982004111159959, -2.000000000000000888 ) ) ;
#14600 = CARTESIAN_POINT ( 'NONE',  ( 0.02531912748464718033, -14.46287784598619020, 2.311161484776505404 ) ) ;
#14601 = ORIENTED_EDGE ( 'NONE', *, *, #9356, .F. ) ;
#14602 = ORIENTED_EDGE ( 'NONE', *, *, #6671, .F. ) ;
#14603 = CARTESIAN_POINT ( 'NONE',  ( 2.789999999999999147, -16.37294372382871188, 18.55949924794887096 ) ) ;
#14604 = CARTESIAN_POINT ( 'NONE',  ( -14.40394475573012301, -13.79473832354794993, 16.99999999999999645 ) ) ;
#14605 = CARTESIAN_POINT ( 'NONE',  ( 2.789999999999999147, -19.64056340710884996, 14.55412442567610931 ) ) ;
#14606 = CARTESIAN_POINT ( 'NONE',  ( 2.789999999999999147, 1.948757464274172513, 13.87420763704361804 ) ) ;
#14607 = CARTESIAN_POINT ( 'NONE',  ( 1.039999999999996483, 17.29145405592695539, -4.835383649608292700 ) ) ;
#14608 = AXIS2_PLACEMENT_3D ( 'NONE', #12644, #10420, #13878 ) ;
#14609 = AXIS2_PLACEMENT_3D ( 'NONE', #2090, #13928, #6782 ) ;
#14610 = AXIS2_PLACEMENT_3D ( 'NONE', #13364, #13224, #7464 ) ;
#14611 = CYLINDRICAL_SURFACE ( 'NONE', #11282, 2.524999999999995914 ) ;
#14612 =( REPRESENTATION_RELATIONSHIP ('NONE','NONE', #12685, #13067 ) REPRESENTATION_RELATIONSHIP_WITH_TRANSFORMATION ( #11641 )SHAPE_REPRESENTATION_RELATIONSHIP( ) );
#14613 = EDGE_CURVE ( 'NONE', #1296, #6140, #11461, .T. ) ;
#14614 = ORIENTED_EDGE ( 'NONE', *, *, #1277, .T. ) ;
#14615 = B_SPLINE_CURVE_WITH_KNOTS ( 'NONE', 3,
 ( #1848, #12529, #5622, #10145 ),
 .UNSPECIFIED., .F., .F.,
 ( 4, 4 ),
 ( 0.005258214619651957987, 0.005948481662034167325 ),
 .UNSPECIFIED. ) ;
#14616 = CARTESIAN_POINT ( 'NONE',  ( -8.051804217113518143E-16, 5.456805104201102985, 23.69843731927169728 ) ) ;
#14617 = CARTESIAN_POINT ( 'NONE',  ( 14.40394475573011945, -10.79473832354794460, 3.000000000000000000 ) ) ;
#14618 = EDGE_CURVE ( 'NONE', #8930, #9372, #10045, .T. ) ;
#14619 = AXIS2_PLACEMENT_3D ( 'NONE', #6059, #10746, #8506 ) ;
#14620 = VECTOR ( 'NONE', #14503, 1000.000000000000000 ) ;
#14621 = COLOUR_RGB ( '',1.000000000000000000, 0.9490196078431372140, 0.9098039215686274384 ) ;
#14622 = EDGE_CURVE ( 'NONE', #8536, #8896, #13530, .T. ) ;
#14623 = VERTEX_POINT ( 'NONE', #12447 ) ;
#14624 = VERTEX_POINT ( 'NONE', #7914 ) ;
#14625 = ORIENTED_EDGE ( 'NONE', *, *, #7762, .T. ) ;
#14626 = FACE_OUTER_BOUND ( 'NONE', #11106, .T. ) ;
#14627 = ORIENTED_EDGE ( 'NONE', *, *, #9950, .T. ) ;
#14628 = FACE_OUTER_BOUND ( 'NONE', #3393, .T. ) ;
#14629 = DIRECTION ( 'NONE',  ( 0.000000000000000000, 0.000000000000000000, 1.000000000000000000 ) ) ;
#14630 = AXIS2_PLACEMENT_3D ( 'NONE', #4013, #14317, #5114 ) ;
#14631 = EDGE_CURVE ( 'NONE', #3152, #13441, #12915, .T. ) ;
#14632 = ORIENTED_EDGE ( 'NONE', *, *, #14408, .F. ) ;
#14633 = ADVANCED_FACE ( 'NONE', ( #5689 ), #13901, .T. ) ;
#14634 = CARTESIAN_POINT ( 'NONE',  ( -20.63749999999999929, 0.000000000000000000, 0.000000000000000000 ) ) ;
#14635 = CARTESIAN_POINT ( 'NONE',  ( 2.789999999999999147, 7.739906618939707883, 13.40591150984229252 ) ) ;
#14636 = CARTESIAN_POINT ( 'NONE',  ( 0.1869148386924337490, 14.83319344613230584, 5.279841123861332086 ) ) ;
#14637 = CARTESIAN_POINT ( 'NONE',  ( 1.039999999999997371, 25.12109765559653596, 12.52377138324232675 ) ) ;
#14638 = DIRECTION ( 'NONE',  ( 0.000000000000000000, 0.000000000000000000, 1.000000000000000000 ) ) ;
#14639 = VERTEX_POINT ( 'NONE', #13031 ) ;
#14640 = CARTESIAN_POINT ( 'NONE',  ( 0.02436607992776064838, 12.59161484032912171, 21.30679549418635688 ) ) ;
#14641 = CIRCLE ( 'NONE', #3835, 2.524999999999995914 ) ;
#14642 = CARTESIAN_POINT ( 'NONE',  ( 2.789999999999999147, -14.59528211760000005, 5.279841123860814278 ) ) ;
#14643 = B_SPLINE_CURVE_WITH_KNOTS ( 'NONE', 3,
 ( #7676, #11287, #9064, #8976 ),
 .UNSPECIFIED., .F., .F.,
 ( 4, 4 ),
 ( 1.981826382900813409E-07, 0.0006887856082032216450 ),
 .UNSPECIFIED. ) ;
#14644 = ORIENTED_EDGE ( 'NONE', *, *, #11818, .T. ) ;
#14645 = ORIENTED_EDGE ( 'NONE', *, *, #1290, .T. ) ;
#14646 = LINE ( 'NONE', #13838, #1172 ) ;
#14647 = DIRECTION ( 'NONE',  ( 0.000000000000000000, 1.374038396813314756E-15, -1.000000000000000000 ) ) ;
#14648 = EDGE_CURVE ( 'NONE', #12150, #6879, #9743, .T. ) ;
#14649 = CARTESIAN_POINT ( 'NONE',  ( 1.249999999999998002, 4.100000000000000533, 0.000000000000000000 ) ) ;
#14650 = EDGE_CURVE ( 'NONE', #418, #2971, #8354, .T. ) ;
#14651 = EDGE_CURVE ( 'NONE', #1007, #9176, #3590, .T. ) ;
#14652 = AXIS2_PLACEMENT_3D ( 'NONE', #5079, #7450, #13350 ) ;
#14653 = CARTESIAN_POINT ( 'NONE',  ( -19.40394475573012301, -16.79473832354794993, 22.00000000000000000 ) ) ;
#14654 = EDGE_LOOP ( 'NONE', ( #4839, #9745, #14294, #10405 ) ) ;
#14655 = CARTESIAN_POINT ( 'NONE',  ( 0.1855655959470679794, 19.17825124759777822, 17.45907811351462158 ) ) ;
#14656 = CARTESIAN_POINT ( 'NONE',  ( -19.40394475573011590, -4.794738323547945491, 12.00000000000000000 ) ) ;
#14657 = CIRCLE ( 'NONE', #1392, 11.66666666666667318 ) ;
#14658 = ORIENTED_EDGE ( 'NONE', *, *, #3790, .T. ) ;
#14659 = DIRECTION ( 'NONE',  ( 0.000000000000000000, 0.000000000000000000, 1.000000000000000000 ) ) ;
#14660 = EDGE_CURVE ( 'NONE', #7166, #1439, #2368, .T. ) ;
#14661 = ORIENTED_EDGE ( 'NONE', *, *, #1247, .T. ) ;
#14662 = ORIENTED_EDGE ( 'NONE', *, *, #14894, .F. ) ;
#14663 = AXIS2_PLACEMENT_3D ( 'NONE', #4290, #13583, #13744 ) ;
#14664 = EDGE_LOOP ( 'NONE', ( #12338, #10043, #8745, #10797 ) ) ;
#14665 = CARTESIAN_POINT ( 'NONE',  ( 0.07181525068722571792, -25.22524549359951962, 2.576941577947320372 ) ) ;
#14666 = CARTESIAN_POINT ( 'NONE',  ( 0.5279272304333949561, 11.57956866523252870, -24.43806413951663004 ) ) ;
#14667 = AXIS2_PLACEMENT_3D ( 'NONE', #14911, #12445, #7840 ) ;
#14668 = LINE ( 'NONE', #9740, #12194 ) ;
#14669 = LINE ( 'NONE', #3052, #9204 ) ;
#14670 = CIRCLE ( 'NONE', #907, 17.95481323787947403 ) ;
#14671 = CARTESIAN_POINT ( 'NONE',  ( 2.789999999999999147, 7.909232158575156824, -24.34211360614291664 ) ) ;
#14672 = CIRCLE ( 'NONE', #5112, 4.000000000000003553 ) ;
#14673 = CARTESIAN_POINT ( 'NONE',  ( 0.000000000000000000, 0.000000000000000000, 0.000000000000000000 ) ) ;
#14674 = CARTESIAN_POINT ( 'NONE',  ( 0.000000000000000000, 0.000000000000000000, -10.00000000000000000 ) ) ;
#14675 = ORIENTED_EDGE ( 'NONE', *, *, #6921, .F. ) ;
#14676 = DIRECTION ( 'NONE',  ( -1.000000000000000000, 0.000000000000000000, 0.000000000000000000 ) ) ;
#14677 = DIRECTION ( 'NONE',  ( -5.339417856040273846E-17, -1.063174570779084847E-17, 1.000000000000000000 ) ) ;
#14678 = CARTESIAN_POINT ( 'NONE',  ( 2.631259771887293653, -22.38003579136350396, 12.81821841996065636 ) ) ;
#14679 = EDGE_CURVE ( 'NONE', #367, #5551, #10526, .T. ) ;
#14680 = ORIENTED_EDGE ( 'NONE', *, *, #14005, .T. ) ;
#14681 = AXIS2_PLACEMENT_3D ( 'NONE', #1672, #12269, #2677 ) ;
#14682 =( GEOMETRIC_REPRESENTATION_CONTEXT ( 3 ) GLOBAL_UNCERTAINTY_ASSIGNED_CONTEXT ( ( #7477 ) ) GLOBAL_UNIT_ASSIGNED_CONTEXT ( ( #3886, #5279, #8567 ) ) REPRESENTATION_CONTEXT ( 'NONE', 'WORKASPACE' ) );
#14683 = CARTESIAN_POINT ( 'NONE',  ( 2.337784062669568730, 16.32199768300068499, -3.429166897524400071 ) ) ;
#14685 = AXIS2_PLACEMENT_3D ( 'NONE', #6886, #6592, #12570 ) ;
#14684 = CARTESIAN_POINT ( 'NONE',  ( 56.98919079003883326, 3.953582723775848962, 4.000000000000000000 ) ) ;
#14686 = ORIENTED_EDGE ( 'NONE', *, *, #7651, .F. ) ;
#14687 = AXIS2_PLACEMENT_3D ( 'NONE', #8624, #7338, #9707 ) ;
#14688 = ORIENTED_EDGE ( 'NONE', *, *, #1569, .T. ) ;
#14689 = DIRECTION ( 'NONE',  ( 0.000000000000000000, 0.3090169943749544457, -0.9510565162951513107 ) ) ;
#14690 = CARTESIAN_POINT ( 'NONE',  ( 2.257825462012207129, -12.96514671151749631, -23.74442027961374890 ) ) ;
#14691 = DIRECTION ( 'NONE',  ( 0.000000000000000000, -6.870191984066566880E-16, -1.000000000000000000 ) ) ;
#14692 = LINE ( 'NONE', #14917, #12860 ) ;
#14693 = VECTOR ( 'NONE', #4032, 1000.000000000000000 ) ;
#14694 = DIRECTION ( 'NONE',  ( 0.000000000000000000, 0.000000000000000000, -1.000000000000000000 ) ) ;
#14695 = EDGE_CURVE ( 'NONE', #2817, #6170, #4692, .T. ) ;
#14696 = ORIENTED_EDGE ( 'NONE', *, *, #1603, .F. ) ;
#14697 = CARTESIAN_POINT ( 'NONE',  ( 0.02531912748464674665, -11.36963888406694068, 9.232963481057725019 ) ) ;
#14698 = VECTOR ( 'NONE', #5227, 1000.000000000000000 ) ;
#14699 = VECTOR ( 'NONE', #5739, 1000.000000000000000 ) ;
#14700 = DIRECTION ( 'NONE',  ( 1.000000000000000000, 0.000000000000000000, -0.000000000000000000 ) ) ;
#14701 = ORIENTED_EDGE ( 'NONE', *, *, #11826, .T. ) ;
#14702 = B_SPLINE_CURVE_WITH_KNOTS ( 'NONE', 3,
 ( #8191, #5902, #12869, #33 ),
 .UNSPECIFIED., .F., .F.,
 ( 4, 4 ),
 ( 0.005123742438166227833, 0.005814376014856856636 ),
 .UNSPECIFIED. ) ;
#14703 = ORIENTED_EDGE ( 'NONE', *, *, #13497, .F. ) ;
#14704 = ORIENTED_EDGE ( 'NONE', *, *, #8071, .T. ) ;
#14705 = ORIENTED_EDGE ( 'NONE', *, *, #8488, .F. ) ;
#14706 = DIRECTION ( 'NONE',  ( 0.000000000000000000, 0.000000000000000000, 1.000000000000000000 ) ) ;
#14707 = EDGE_CURVE ( 'NONE', #5314, #2246, #12973, .T. ) ;
#14708 =( NAMED_UNIT ( * ) SI_UNIT ( $, .STERADIAN. ) SOLID_ANGLE_UNIT ( ) );
#14709 = APPLICATION_CONTEXT ( 'automotive_design' ) ;
#14710 = TOROIDAL_SURFACE ( 'NONE', #4852, 14.01039946648074341, 8.000000000000000000 ) ;
#14711 = AXIS2_PLACEMENT_3D ( 'NONE', #15048, #10058, #4219 ) ;
#14712 = EDGE_CURVE ( 'NONE', #6698, #3271, #9429, .T. ) ;
#14713 = UNCERTAINTY_MEASURE_WITH_UNIT (LENGTH_MEASURE( 1.000000000000000082E-05 ), #8919, 'distance_accuracy_value', 'NONE');
#14714 = CYLINDRICAL_SURFACE ( 'NONE', #9556, 8.400000000000000355 ) ;
#14715 = DIRECTION ( 'NONE',  ( 0.000000000000000000, 0.000000000000000000, 1.000000000000000000 ) ) ;
#14716 = ORIENTED_EDGE ( 'NONE', *, *, #7270, .F. ) ;
#14717 = CARTESIAN_POINT ( 'NONE',  ( 2.789999999999999147, 0.000000000000000000, 0.000000000000000000 ) ) ;
#14718 = CARTESIAN_POINT ( 'NONE',  ( 0.2393399843456231746, 15.07093484180037812, 5.269646308239136268 ) ) ;
#14719 = VECTOR ( 'NONE', #7189, 1000.000000000000000 ) ;
#14720 = CARTESIAN_POINT ( 'NONE',  ( 2.789999999999999147, 21.30679549418631780, 12.59161484032919986 ) ) ;
#14721 = ORIENTED_EDGE ( 'NONE', *, *, #4383, .F. ) ;
#14722 = CARTESIAN_POINT ( 'NONE',  ( 0.01819315239479611657, 13.58898324715688588, -5.219858754686030444 ) ) ;
#14723 = LINE ( 'NONE', #7797, #14103 ) ;
#14724 = EDGE_LOOP ( 'NONE', ( #4335, #4092, #1996, #1241, #2838, #14721, #656 ) ) ;
#14725 = ORIENTED_EDGE ( 'NONE', *, *, #2318, .F. ) ;
#14726 = DIRECTION ( 'NONE',  ( 1.000000000000000000, 0.000000000000000000, 0.000000000000000000 ) ) ;
#14727 = CARTESIAN_POINT ( 'NONE',  ( 0.02436607992776758727, 24.15498966839963302, 5.391175441198700291 ) ) ;
#14728 = VECTOR ( 'NONE', #2845, 1000.000000000000000 ) ;
#14729 = EDGE_CURVE ( 'NONE', #1373, #383, #4850, .T. ) ;
#14730 = FACE_OUTER_BOUND ( 'NONE', #13638, .T. ) ;
#14731 = VERTEX_POINT ( 'NONE', #14356 ) ;
#14732 = CARTESIAN_POINT ( 'NONE',  ( 0.000000000000000000, 0.000000000000000000, 0.000000000000000000 ) ) ;
#14733 = FACE_OUTER_BOUND ( 'NONE', #11894, .T. ) ;
#14734 = EDGE_LOOP ( 'NONE', ( #8385, #7169, #9691, #11840, #11401, #13359, #7813, #14566 ) ) ;
#14735 = CARTESIAN_POINT ( 'NONE',  ( 0.07186811453410731076, 16.91241718342026346, -18.89333555428536826 ) ) ;
#14736 = CARTESIAN_POINT ( 'NONE',  ( -16.80212006966224791, -13.74240776967763900, 0.7999999999999960476 ) ) ;
#14737 = ORIENTED_EDGE ( 'NONE', *, *, #14561, .F. ) ;
#14738 = VECTOR ( 'NONE', #12865, 1000.000000000000114 ) ;
#14739 = VERTEX_POINT ( 'NONE', #7134 ) ;
#14740 = EDGE_CURVE ( 'NONE', #3394, #495, #6132, .T. ) ;
#14741 = EDGE_CURVE ( 'NONE', #14210, #5125, #10815, .T. ) ;
#14742 = ORIENTED_EDGE ( 'NONE', *, *, #972, .T. ) ;
#14743 = DIRECTION ( 'NONE',  ( -0.4036950204470263204, 0.9148936170212770280, 0.000000000000000000 ) ) ;
#14744 = CYLINDRICAL_SURFACE ( 'NONE', #1674, 2.524999999999999467 ) ;
#14745 = CARTESIAN_POINT ( 'NONE',  ( 13.28797974610715116, -21.11867004231547540, 4.000000000000000000 ) ) ;
#14746 = CARTESIAN_POINT ( 'NONE',  ( 2.765633920072235963, -24.63872515616080960, -2.336989772644527008 ) ) ;
#14747 = ITEM_DEFINED_TRANSFORMATION ( 'NONE', 'NONE', #6474,  #1376 ) ;
#14748 = DIRECTION ( 'NONE',  ( 0.000000000000000000, 0.000000000000000000, 1.000000000000000000 ) ) ;
#14749 = CARTESIAN_POINT ( 'NONE',  ( 2.789999999999999147, -15.74360496233368245, -18.28042085475295409 ) ) ;
#14750 = CARTESIAN_POINT ( 'NONE',  ( 0.000000000000000000, 0.000000000000000000, -0.8000000000000000444 ) ) ;
#14751 = ORIENTED_EDGE ( 'NONE', *, *, #9304, .T. ) ;
#14752 = CARTESIAN_POINT ( 'NONE',  ( 0.000000000000000000, 0.000000000000000000, 5.500000000000000000 ) ) ;
#14753 = DIRECTION ( 'NONE',  ( -0.9148936170212769170, -0.4036950204470262649, 0.000000000000000000 ) ) ;
#14754 = EDGE_CURVE ( 'NONE', #960, #10087, #3742, .T. ) ;
#14755 = DIRECTION ( 'NONE',  ( -1.000000000000000000, -0.000000000000000000, -0.000000000000000000 ) ) ;
#14756 = EDGE_CURVE ( 'NONE', #12602, #8463, #10593, .T. ) ;
#14757 = ORIENTED_EDGE ( 'NONE', *, *, #8807, .F. ) ;
#14758 = ADVANCED_FACE ( 'NONE', ( #11877 ), #8420, .F. ) ;
#14759 = DIRECTION ( 'NONE',  ( -0.000000000000000000, -0.000000000000000000, 1.000000000000000000 ) ) ;
#14760 = DIRECTION ( 'NONE',  ( 1.445602896647338917E-16, -1.000000000000000000, -0.000000000000000000 ) ) ;
#14761 = EDGE_LOOP ( 'NONE', ( #3685, #14658, #9469, #15135, #6766, #7093, #1261, #8212 ) ) ;
#14762 = ORIENTED_EDGE ( 'NONE', *, *, #10881, .T. ) ;
#14763 = CARTESIAN_POINT ( 'NONE',  ( 101.4858053992934401, 0.9022481406819604643, 2.999999999999999112 ) ) ;
#14764 = CARTESIAN_POINT ( 'NONE',  ( 0.9041604829517136954, -17.20101185193997395, -4.239993951493388202 ) ) ;
#14765 = CARTESIAN_POINT ( 'NONE',  ( -0.1713913650100259145, 0.000000000000000000, 5.575000000000000178 ) ) ;
#14766 = CARTESIAN_POINT ( 'NONE',  ( 91.46153288930040048, 16.46030115554384565, 7.000000000000000000 ) ) ;
#14767 = EDGE_CURVE ( 'NONE', #1724, #4526, #156, .T. ) ;
#14768 = DIRECTION ( 'NONE',  ( 0.000000000000000000, 0.000000000000000000, 1.000000000000000000 ) ) ;
#14769 = CARTESIAN_POINT ( 'NONE',  ( 2.789999999999999147, 7.739906618939895289, -13.40591150984218416 ) ) ;
#14770 = ORIENTED_EDGE ( 'NONE', *, *, #6912, .F. ) ;
#14771 = CARTESIAN_POINT ( 'NONE',  ( -14.40394475573011945, -10.79473832354794283, -3.000000000000000000 ) ) ;
#14772 = CARTESIAN_POINT ( 'NONE',  ( 2.789999999999999147, 5.391175441198956086, -24.15498966839956907 ) ) ;
#14773 = ORIENTED_EDGE ( 'NONE', *, *, #12490, .F. ) ;
#14774 = ORIENTED_EDGE ( 'NONE', *, *, #12278, .F. ) ;
#14775 = ORIENTED_EDGE ( 'NONE', *, *, #4968, .T. ) ;
#14776 = EDGE_LOOP ( 'NONE', ( #12904, #1026, #8593, #10339, #925, #3583 ) ) ;
#14777 = FACE_OUTER_BOUND ( 'NONE', #12978, .T. ) ;
#14778 = FACE_OUTER_BOUND ( 'NONE', #1636, .T. ) ;
#14779 = DIRECTION ( 'NONE',  ( -1.000000000000000000, 5.782411586589353694E-16, 0.000000000000000000 ) ) ;
#14780 = CARTESIAN_POINT ( 'NONE',  ( 2.789999999999999147, 0.000000000000000000, 0.000000000000000000 ) ) ;
#14781 = EDGE_CURVE ( 'NONE', #4617, #4474, #9009, .T. ) ;
#14782 = ORIENTED_EDGE ( 'NONE', *, *, #3317, .F. ) ;
#14783 = DIRECTION ( 'NONE',  ( 1.000000000000000000, 0.000000000000000000, 0.000000000000000000 ) ) ;
#14784 = FACE_OUTER_BOUND ( 'NONE', #14554, .T. ) ;
#14785 = DIRECTION ( 'NONE',  ( 0.000000000000000000, 0.000000000000000000, 1.000000000000000000 ) ) ;
#14786 = AXIS2_PLACEMENT_3D ( 'NONE', #2984, #10349, #7747 ) ;
#14787 = CARTESIAN_POINT ( 'NONE',  ( 0.6180618139040615633, -23.93436800624301242, 12.96259772325168314 ) ) ;
#14788 = EDGE_CURVE ( 'NONE', #3479, #2220, #12962, .T. ) ;
#14789 = ORIENTED_EDGE ( 'NONE', *, *, #2308, .F. ) ;
#14790 = FACE_OUTER_BOUND ( 'NONE', #8602, .T. ) ;
#14791 = LINE ( 'NONE', #2955, #10672 ) ;
#14792 = VERTEX_POINT ( 'NONE', #1281 ) ;
#14793 = VERTEX_POINT ( 'NONE', #10660 ) ;
#14794 = CARTESIAN_POINT ( 'NONE',  ( 2.765633920072235075, 24.63872515616082737, -2.336989772644355590 ) ) ;
#14795 = VECTOR ( 'NONE', #1930, 1000.000000000000227 ) ;
#14796 = AXIS2_PLACEMENT_3D ( 'NONE', #10037, #7948, #1973 ) ;
#14797 = CARTESIAN_POINT ( 'NONE',  ( 2.789999999999999147, 12.98979500319694047, 5.249430348645800493 ) ) ;
#14798 = ORIENTED_EDGE ( 'NONE', *, *, #6108, .F. ) ;
#14799 = CARTESIAN_POINT ( 'NONE',  ( 2.764680872513682441, -2.311161484776455222, -14.46287784598619908 ) ) ;
#14800 = ORIENTED_EDGE ( 'NONE', *, *, #14468, .F. ) ;
#14801 = CARTESIAN_POINT ( 'NONE',  ( 1.039999999999995595, 20.02152543075345648, 19.67366047555537278 ) ) ;
#14802 = FACE_OUTER_BOUND ( 'NONE', #15000, .T. ) ;
#14803 = VERTEX_POINT ( 'NONE', #5974 ) ;
#14804 = DIRECTION ( 'NONE',  ( -0.000000000000000000, -0.000000000000000000, 1.000000000000000000 ) ) ;
#14805 = ADVANCED_FACE ( 'NONE', ( #12107 ), #12192, .F. ) ;
#14806 = AXIS2_PLACEMENT_3D ( 'NONE', #14407, #14492, #6405 ) ;
#14807 = CYLINDRICAL_SURFACE ( 'NONE', #12177, 8.400000000000000355 ) ;
#14808 = ORIENTED_EDGE ( 'NONE', *, *, #12553, .T. ) ;
#14809 = EDGE_CURVE ( 'NONE', #2825, #8456, #12043, .T. ) ;
#14810 = VERTEX_POINT ( 'NONE', #1594 ) ;
#14811 = B_SPLINE_CURVE_WITH_KNOTS ( 'NONE', 3,
 ( #4076, #7615, #14690, #4159, #10907, #12291 ),
 .UNSPECIFIED., .F., .F.,
 ( 4, 2, 4 ),
 ( 4.462636695616422376E-07, 0.001879885036799763083, 0.003759323809929964420 ),
 .UNSPECIFIED. ) ;
#14812 = DIRECTION ( 'NONE',  ( 1.000000000000000000, -0.000000000000000000, 0.000000000000000000 ) ) ;
#14813 = FACE_OUTER_BOUND ( 'NONE', #5557, .T. ) ;
#14814 = LINE ( 'NONE', #8960, #4122 ) ;
#14815 = DIRECTION ( 'NONE',  ( -1.000000000000000000, 0.000000000000000000, 0.000000000000000000 ) ) ;
#14816 = DIRECTION ( 'NONE',  ( -1.000000000000000000, 0.000000000000000000, 0.000000000000000000 ) ) ;
#14817 = CARTESIAN_POINT ( 'NONE',  ( 2.783068930044319877, -16.17493693894864393, -18.43696893154776006 ) ) ;
#14818 = DIRECTION ( 'NONE',  ( 1.000000000000000000, 0.000000000000000000, 0.000000000000000000 ) ) ;
#14819 = PRODUCT_RELATED_PRODUCT_CATEGORY ( 'part', '', ( #2480 ) ) ;
#14820 = EDGE_CURVE ( 'NONE', #2289, #6867, #12456, .T. ) ;
#14821 = VERTEX_POINT ( 'NONE', #7595 ) ;
#14822 = DIRECTION ( 'NONE',  ( -0.8893705212896292345, 0.4571871344001418036, 0.000000000000000000 ) ) ;
#14823 = EDGE_CURVE ( 'NONE', #14477, #1275, #14668, .T. ) ;
#14824 = CARTESIAN_POINT ( 'NONE',  ( 2.789999999999999147, 24.34211360614300190, 7.909232158574900140 ) ) ;
#14825 = CARTESIAN_POINT ( 'NONE',  ( -0.4472135954999577612, 0.000000000000000000, 0.000000000000000000 ) ) ;
#14826 = ORIENTED_EDGE ( 'NONE', *, *, #2598, .F. ) ;
#14827 = DIRECTION ( 'NONE',  ( 0.000000000000000000, 0.000000000000000000, 1.000000000000000000 ) ) ;
#14828 = ORIENTED_EDGE ( 'NONE', *, *, #14233, .F. ) ;
#14829 = ORIENTED_EDGE ( 'NONE', *, *, #7383, .T. ) ;
#14830 = CARTESIAN_POINT ( 'NONE',  ( 1.749999999999998002, 0.000000000000000000, 0.000000000000000000 ) ) ;
#14831 = CARTESIAN_POINT ( 'NONE',  ( 2.771806847605205792, -13.58898324715675976, -5.219858754686313773 ) ) ;
#14832 = CARTESIAN_POINT ( 'NONE',  ( 2.790000000000061764, 2.096282088614963346, -14.05326139264725427 ) ) ;
#14833 = CARTESIAN_POINT ( 'NONE',  ( 13.78117670802322259, -24.07785181381190753, -2.000000000000000000 ) ) ;
#14834 = CARTESIAN_POINT ( 'NONE',  ( -10.00000000000000000, 0.000000000000000000, 0.000000000000000000 ) ) ;
#14835 = ADVANCED_FACE ( 'NONE', ( #577 ), #5296, .T. ) ;
#14836 = B_SPLINE_CURVE_WITH_KNOTS ( 'NONE', 3,
 ( #10945, #8486, #13257, #3889 ),
 .UNSPECIFIED., .F., .F.,
 ( 4, 4 ),
 ( 0.005258110598983608240, 0.005948376585272727862 ),
 .UNSPECIFIED. ) ;
#14837 = DIRECTION ( 'NONE',  ( -1.000000000000000000, -0.000000000000000000, -0.000000000000000000 ) ) ;
#14838 = CARTESIAN_POINT ( 'NONE',  ( 0.007327564474062031770, -9.044896821682122834, -11.23174270417338505 ) ) ;
#14839 = EDGE_CURVE ( 'NONE', #11986, #4864, #1168, .T. ) ;
#14840 = ORIENTED_EDGE ( 'NONE', *, *, #5456, .F. ) ;
#14841 = CARTESIAN_POINT ( 'NONE',  ( 2.764680872515352217, 14.46287784598617243, 2.311161484776605324 ) ) ;
#14842 = CIRCLE ( 'NONE', #3049, 0.1000000000000011297 ) ;
#14843 = AXIS2_PLACEMENT_3D ( 'NONE', #847, #4628, #8077 ) ;
#14844 = B_SPLINE_CURVE_WITH_KNOTS ( 'NONE', 3,
 ( #9818, #13503, #11954, #6130 ),
 .UNSPECIFIED., .F., .F.,
 ( 4, 4 ),
 ( 0.005123742438166223497, 0.005540500595652399218 ),
 .UNSPECIFIED. ) ;
#14845 = CARTESIAN_POINT ( 'NONE',  ( 0.000000000000000000, 6.123233995736766282E-16, -5.000000000000000000 ) ) ;
#14846 = EDGE_LOOP ( 'NONE', ( #6417, #3469, #10093, #4340 ) ) ;
#14847 = EDGE_CURVE ( 'NONE', #11410, #8704, #7487, .T. ) ;
#14848 = EDGE_LOOP ( 'NONE', ( #10626, #279, #8871, #7717 ) ) ;
#14849 = VERTEX_POINT ( 'NONE', #4055 ) ;
#14850 = ORIENTED_EDGE ( 'NONE', *, *, #11899, .F. ) ;
#14851 = CARTESIAN_POINT ( 'NONE',  ( 2.718184749312774873, 25.22524549359950541, 2.576941577947493567 ) ) ;
#14852 = AXIS2_PLACEMENT_3D ( 'NONE', #14996, #4386, #10443 ) ;
#14853 = SURFACE_SIDE_STYLE ('',( #9003 ) ) ;
#14854 = VECTOR ( 'NONE', #1059, 1000.000000000000000 ) ;
#14855 = AXIS2_PLACEMENT_3D ( 'NONE', #5923, #9440, #7298 ) ;
#14856 = CYLINDRICAL_SURFACE ( 'NONE', #10551, 5.000000000000000888 ) ;
#14857 = EDGE_LOOP ( 'NONE', ( #2965, #9140, #64, #7223 ) ) ;
#14859 = DIRECTION ( 'NONE',  ( -1.000000000000000000, 0.000000000000000000, 0.000000000000000000 ) ) ;
#14858 = AXIS2_PLACEMENT_3D ( 'NONE', #3606, #15156, #4632 ) ;
#14860 = CARTESIAN_POINT ( 'NONE',  ( 2.790000000000000036, -23.69843731927165109, -5.456805104201351675 ) ) ;
#14861 = CARTESIAN_POINT ( 'NONE',  ( 1.039999999999997593, 0.000000000000000000, 0.000000000000000000 ) ) ;
#14862 = AXIS2_PLACEMENT_3D ( 'NONE', #7474, #4249, #8924 ) ;
#14863 = CARTESIAN_POINT ( 'NONE',  ( 0.06562551705663710599, -21.84204283372370625, 12.72258903105631234 ) ) ;
#14864 = ORIENTED_EDGE ( 'NONE', *, *, #9318, .F. ) ;
#14865 = DIRECTION ( 'NONE',  ( -1.000000000000000000, 0.000000000000000000, 0.000000000000000000 ) ) ;
#14866 = LINE ( 'NONE', #791, #9936 ) ;
#14867 = ORIENTED_EDGE ( 'NONE', *, *, #13512, .T. ) ;
#14868 = EDGE_LOOP ( 'NONE', ( #4827, #8634, #8284, #11537 ) ) ;
#14869 = CIRCLE ( 'NONE', #7005, 1.999999999999998446 ) ;
#14870 = AXIS2_PLACEMENT_3D ( 'NONE', #4489, #9326, #3255 ) ;
#14871 = CARTESIAN_POINT ( 'NONE',  ( 0.000000000000000000, 0.000000000000000000, 0.000000000000000000 ) ) ;
#14872 = ORIENTED_EDGE ( 'NONE', *, *, #9233, .F. ) ;
#14873 = CARTESIAN_POINT ( 'NONE',  ( -14.40394475573011945, -10.79473832354794460, -3.799999999999999822 ) ) ;
#14874 = EDGE_CURVE ( 'NONE', #4008, #5666, #2748, .T. ) ;
#14875 = ORIENTED_EDGE ( 'NONE', *, *, #8159, .T. ) ;
#14876 = DIRECTION ( 'NONE',  ( 0.000000000000000000, 0.000000000000000000, 1.000000000000000000 ) ) ;
#14877 = DIRECTION ( 'NONE',  ( -1.000000000000000000, 0.000000000000000000, 0.000000000000000000 ) ) ;
#14878 = ORIENTED_EDGE ( 'NONE', *, *, #1816, .T. ) ;
#14879 = VECTOR ( 'NONE', #9982, 1000.000000000000000 ) ;
#14880 = DIRECTION ( 'NONE',  ( -1.000000000000000000, 0.000000000000000000, 0.000000000000000000 ) ) ;
#14881 = DIRECTION ( 'NONE',  ( 1.000000000000000000, 0.000000000000000000, 0.000000000000000000 ) ) ;
#14882 = ORIENTED_EDGE ( 'NONE', *, *, #3274, .T. ) ;
#14883 = EDGE_LOOP ( 'NONE', ( #302, #5835, #5004, #5385, #1628, #806, #3840 ) ) ;
#14884 = CARTESIAN_POINT ( 'NONE',  ( 0.000000000000000000, -24.04302995059967429, 1.991882183130232242 ) ) ;
#14885 = CARTESIAN_POINT ( 'NONE',  ( -10.00000000000000000, 0.000000000000000000, 0.000000000000000000 ) ) ;
#14886 = EDGE_CURVE ( 'NONE', #3346, #4276, #6069, .T. ) ;
#14887 = AXIS2_PLACEMENT_3D ( 'NONE', #13909, #6917, #11594 ) ;
#14888 = B_SPLINE_CURVE_WITH_KNOTS ( 'NONE', 3,
 ( #4211, #13649, #11412, #5516 ),
 .UNSPECIFIED., .F., .F.,
 ( 4, 4 ),
 ( 0.002880534149780641148, 0.003796793755617278946 ),
 .UNSPECIFIED. ) ;
#14889 = DIRECTION ( 'NONE',  ( 1.000000000000000000, 0.000000000000000000, 0.000000000000000000 ) ) ;
#14890 = CARTESIAN_POINT ( 'NONE',  ( 61.44848940674400239, 29.65768221419895667, 2.000000000000000000 ) ) ;
#14891 = ITEM_DEFINED_TRANSFORMATION ( 'NONE', 'NONE', #2787,  #1376 ) ;
#14892 = CARTESIAN_POINT ( 'NONE',  ( 2.789999999999999147, 5.229914364928351489, 13.68080036884350292 ) ) ;
#14893 = VECTOR ( 'NONE', #2835, 1000.000000000000114 ) ;
#14894 = EDGE_CURVE ( 'NONE', #6657, #13931, #1157, .T. ) ;
#14895 =( GEOMETRIC_REPRESENTATION_CONTEXT ( 3 ) GLOBAL_UNCERTAINTY_ASSIGNED_CONTEXT ( ( #14713 ) ) GLOBAL_UNIT_ASSIGNED_CONTEXT ( ( #8919, #7924, #10152 ) ) REPRESENTATION_CONTEXT ( 'NONE', 'WORKASPACE' ) );
#14896 = CARTESIAN_POINT ( 'NONE',  ( 0.9999999999999997780, -6.008326913195983998, -0.8000000000000000444 ) ) ;
#14897 = EDGE_LOOP ( 'NONE', ( #6802, #11733, #1668, #11363 ) ) ;
#14898 = FACE_OUTER_BOUND ( 'NONE', #4751, .T. ) ;
#14899 = CARTESIAN_POINT ( 'NONE',  ( 1.039999999999997593, 0.000000000000000000, 0.000000000000000000 ) ) ;
#14900 = EDGE_CURVE ( 'NONE', #1922, #14197, #14670, .T. ) ;
#14901 = CARTESIAN_POINT ( 'NONE',  ( 2.789999999999999147, -9.232963481057685939, -11.36963888406697087 ) ) ;
#14902 = AXIS2_PLACEMENT_3D ( 'NONE', #14825, #4450, #3064 ) ;
#14903 = VECTOR ( 'NONE', #4945, 1000.000000000000114 ) ;
#14904 = EDGE_LOOP ( 'NONE', ( #9253, #14006, #7531, #14909 ) ) ;
#14905 =( REPRESENTATION_RELATIONSHIP ('NONE','NONE', #12685, #7891 ) REPRESENTATION_RELATIONSHIP_WITH_TRANSFORMATION ( #14977 )SHAPE_REPRESENTATION_RELATIONSHIP( ) );
#14906 = DIRECTION ( 'NONE',  ( -1.000000000000000000, -0.000000000000000000, 0.000000000000000000 ) ) ;
#14907 = CARTESIAN_POINT ( 'NONE',  ( 2.789999999999999147, -20.62201879784921843, 12.52067188844344336 ) ) ;
#14908 = ORIENTED_EDGE ( 'NONE', *, *, #8873, .T. ) ;
#14909 = ORIENTED_EDGE ( 'NONE', *, *, #6559, .F. ) ;
#14910 = AXIS2_PLACEMENT_3D ( 'NONE', #5220, #8585, #2820 ) ;
#14911 = CARTESIAN_POINT ( 'NONE',  ( 93.49175023922396122, 0.6585002008270834928, 2.999999999999999112 ) ) ;
#14912 = CARTESIAN_POINT ( 'NONE',  ( 2.031033471609898555, 27.31260702007175567, -3.797536611356413516 ) ) ;
#14913 = EDGE_CURVE ( 'NONE', #12497, #3107, #9967, .T. ) ;
#14914 = ORIENTED_EDGE ( 'NONE', *, *, #2308, .T. ) ;
#14915 = DIRECTION ( 'NONE',  ( 0.000000000000000000, 0.000000000000000000, -1.000000000000000000 ) ) ;
#14916 = DIRECTION ( 'NONE',  ( -1.000000000000000000, 0.000000000000000000, 0.000000000000000000 ) ) ;
#14917 = CARTESIAN_POINT ( 'NONE',  ( -1.000000000000000222, -4.808326913195983821, -0.8000000000000000444 ) ) ;
#14918 = AXIS2_PLACEMENT_3D ( 'NONE', #6349, #13414, #13794 ) ;
#14919 = CARTESIAN_POINT ( 'NONE',  ( 2.789999999999999147, -3.120158876138928505, -14.59528211760005334 ) ) ;
#14920 = CARTESIAN_POINT ( 'NONE',  ( 2.632969638839692372, 22.37100459959346566, 12.81671916049022641 ) ) ;
#14921 = ORIENTED_EDGE ( 'NONE', *, *, #14740, .F. ) ;
#14922 = DIRECTION ( 'NONE',  ( -1.000000000000000000, -0.000000000000000000, -0.000000000000000000 ) ) ;
#14923 = EDGE_CURVE ( 'NONE', #3152, #6903, #427, .T. ) ;
#14924 = AXIS2_PLACEMENT_3D ( 'NONE', #12658, #14992, #13672 ) ;
#14925 = STYLED_ITEM ( 'NONE', ( #1572 ), #14434 ) ;
#14926 = CARTESIAN_POINT ( 'NONE',  ( 2.782672467460655774, -2.217238903388661253, 14.24942254254688478 ) ) ;
#14927 = VECTOR ( 'NONE', #13752, 1000.000000000000000 ) ;
#14928 = EDGE_LOOP ( 'NONE', ( #3795, #9613 ) ) ;
#14929 = AXIS2_PLACEMENT_3D ( 'NONE', #4973, #11859, #5208 ) ;
#14930 = EDGE_CURVE ( 'NONE', #7234, #3861, #1818, .T. ) ;
#14931 = EDGE_LOOP ( 'NONE', ( #535, #15095, #7490, #6884, #14003, #10151 ) ) ;
#14932 = ORIENTED_EDGE ( 'NONE', *, *, #8353, .F. ) ;
#14933 = VERTEX_POINT ( 'NONE', #5151 ) ;
#14934 = CARTESIAN_POINT ( 'NONE',  ( 1.749999999999998002, 27.76164181293051669, 4.147968289691386090 ) ) ;
#14935 = EDGE_CURVE ( 'NONE', #5508, #7872, #2680, .T. ) ;
#14936 = DIRECTION ( 'NONE',  ( 0.000000000000000000, 0.000000000000000000, -1.000000000000000000 ) ) ;
#14937 = ADVANCED_FACE ( 'NONE', ( #6429 ), #6508, .T. ) ;
#14938 = AXIS2_PLACEMENT_3D ( 'NONE', #9802, #9638, #5047 ) ;
#14939 = CARTESIAN_POINT ( 'NONE',  ( 0.006931111373678406143, -9.685942809247212182, 22.53293026234500473 ) ) ;
#14940 = CIRCLE ( 'NONE', #3626, 4.000000000000000888 ) ;
#14941 = AXIS2_PLACEMENT_3D ( 'NONE', #8693, #14132, #11465 ) ;
#14942 = DIRECTION ( 'NONE',  ( -1.000000000000000000, -0.000000000000000000, -0.000000000000000000 ) ) ;
#14943 = ORIENTED_EDGE ( 'NONE', *, *, #1214, .T. ) ;
#14944 = FACE_OUTER_BOUND ( 'NONE', #13753, .T. ) ;
#14945 = DIRECTION ( 'NONE',  ( 0.000000000000000000, 0.000000000000000000, 1.000000000000000000 ) ) ;
#14946 = B_SPLINE_CURVE_WITH_KNOTS ( 'NONE', 3,
 ( #14536, #8670, #9684, #14384 ),
 .UNSPECIFIED., .F., .F.,
 ( 4, 4 ),
 ( 2.159563976372915910E-07, 0.0006916893629248553133 ),
 .UNSPECIFIED. ) ;
#14947 = ADVANCED_FACE ( 'NONE', ( #13803 ), #812, .F. ) ;
#14948 = CARTESIAN_POINT ( 'NONE',  ( 0.3599332783571699279, -23.15620303736534069, 12.90954937922492007 ) ) ;
#14949 = EDGE_CURVE ( 'NONE', #12521, #5940, #8031, .T. ) ;
#14950 = VECTOR ( 'NONE', #9489, 1000.000000000000000 ) ;
#14951 = AXIS2_PLACEMENT_3D ( 'NONE', #11330, #10106, #10261 ) ;
#14952 = VERTEX_POINT ( 'NONE', #7896 ) ;
#14953 = FACE_OUTER_BOUND ( 'NONE', #7857, .T. ) ;
#14954 = CARTESIAN_POINT ( 'NONE',  ( 2.790000000000008473, 11.12243880662625806, -8.842327429718979559 ) ) ;
#14955 = EDGE_CURVE ( 'NONE', #11975, #13815, #7301, .T. ) ;
#14956 = ORIENTED_EDGE ( 'NONE', *, *, #11158, .T. ) ;
#14957 = VERTEX_POINT ( 'NONE', #11342 ) ;
#14958 = DIRECTION ( 'NONE',  ( -0.000000000000000000, -0.000000000000000000, 1.000000000000000000 ) ) ;
#14959 = EDGE_CURVE ( 'NONE', #12416, #3735, #7738, .T. ) ;
#14960 = EDGE_LOOP ( 'NONE', ( #695, #4071, #1798, #13501 ) ) ;
#14961 = DIRECTION ( 'NONE',  ( 0.000000000000000000, 0.000000000000000000, 1.000000000000000000 ) ) ;
#14962 = AXIS2_PLACEMENT_3D ( 'NONE', #8268, #12950, #2439 ) ;
#14963 = AXIS2_PLACEMENT_3D ( 'NONE', #6492, #10179, #648 ) ;
#14964 = AXIS2_PLACEMENT_3D ( 'NONE', #12344, #5299, #2907 ) ;
#14965 = CARTESIAN_POINT ( 'NONE',  ( 0.5279272933715194460, 19.66369668717032937, 18.56460150496945971 ) ) ;
#14966 = DIRECTION ( 'NONE',  ( 1.000000000000000000, 0.000000000000000000, 0.000000000000000000 ) ) ;
#14967 = EDGE_LOOP ( 'NONE', ( #3950, #13385, #3561, #11300 ) ) ;
#14968 = CARTESIAN_POINT ( 'NONE',  ( 0.02436607992776411782, -24.63872515616084513, 2.336989772644183283 ) ) ;
#14969 = ORIENTED_EDGE ( 'NONE', *, *, #11356, .T. ) ;
#14970 = ORIENTED_EDGE ( 'NONE', *, *, #7629, .T. ) ;
#14971 = VERTEX_POINT ( 'NONE', #3050 ) ;
#14972 = CARTESIAN_POINT ( 'NONE',  ( 0.000000000000000000, 1.948757464274177842, 13.87420763704361981 ) ) ;
#14973 = TOROIDAL_SURFACE ( 'NONE', #13986, 14.01039946648074341, 8.000000000000000000 ) ;
#14974 = DIRECTION ( 'NONE',  ( 1.000000000000000000, 0.000000000000000000, 0.000000000000000000 ) ) ;
#14975 = DIRECTION ( 'NONE',  ( 0.000000000000000000, 0.000000000000000000, 1.000000000000000000 ) ) ;
#14976 = DIRECTION ( 'NONE',  ( 0.000000000000000000, 0.000000000000000000, 1.000000000000000000 ) ) ;
#14977 = ITEM_DEFINED_TRANSFORMATION ( 'NONE', 'NONE', #8703,  #1376 ) ;
#14978 = DIRECTION ( 'NONE',  ( -1.000000000000000000, -0.000000000000000000, 0.000000000000000000 ) ) ;
#14979 = CARTESIAN_POINT ( 'NONE',  ( -10.00000000000000000, 0.000000000000000000, 0.000000000000000000 ) ) ;
#14980 = VERTEX_POINT ( 'NONE', #3137 ) ;
#14981 = DIRECTION ( 'NONE',  ( 0.000000000000000000, 0.000000000000000000, 1.000000000000000000 ) ) ;
#14982 = FACE_OUTER_BOUND ( 'NONE', #15065, .T. ) ;
#14983 = ADVANCED_BREP_SHAPE_REPRESENTATION ( '', ( #3717, #1376 ), #12207 ) ;
#14984 = AXIS2_PLACEMENT_3D ( 'NONE', #2524, #7208, #4760 ) ;
#14985 = DIRECTION ( 'NONE',  ( 0.000000000000000000, 0.000000000000000000, 1.000000000000000000 ) ) ;
#14986 = ORIENTED_EDGE ( 'NONE', *, *, #14648, .F. ) ;
#14987 = EDGE_CURVE ( 'NONE', #14792, #1504, #4351, .T. ) ;
#14988 = CARTESIAN_POINT ( 'NONE',  ( 59.43001430450886602, 34.23215029930534570, -2.000000000000000000 ) ) ;
#14989 = CARTESIAN_POINT ( 'NONE',  ( -9.403944755730117677, -16.79473832354794993, 16.99999999999999645 ) ) ;
#14990 = ORIENTED_EDGE ( 'NONE', *, *, #29, .F. ) ;
#14991 = VERTEX_POINT ( 'NONE', #10342 ) ;
#14992 = DIRECTION ( 'NONE',  ( 1.000000000000000000, 0.000000000000000000, 0.000000000000000000 ) ) ;
#14993 = CARTESIAN_POINT ( 'NONE',  ( 1.749999999999998002, 27.76164181293051669, -4.147968289691384314 ) ) ;
#14994 = EDGE_LOOP ( 'NONE', ( #6789, #4015 ) ) ;
#14995 = CARTESIAN_POINT ( 'NONE',  ( 2.765633920072234631, 16.37294372382885044, -18.55949924794875017 ) ) ;
#14996 = CARTESIAN_POINT ( 'NONE',  ( 2.789999999999999147, 7.739906618939895289, -13.40591150984218416 ) ) ;
#14997 = LINE ( 'NONE', #1843, #10178 ) ;
#14998 = CARTESIAN_POINT ( 'NONE',  ( 2.646101151984011857, -14.59528211758545524, 5.279841123860813390 ) ) ;
#14999 = PLANE ( 'NONE',  #3733 ) ;
#15000 = EDGE_LOOP ( 'NONE', ( #12367, #11038, #3973, #2268, #14808, #9896, #13293, #12947, #2040, #5376, #7875, #6902 ) ) ;
#15001 = CARTESIAN_POINT ( 'NONE',  ( 1.039999999999997593, 0.000000000000000000, 0.000000000000000000 ) ) ;
#15002 = PRODUCT_DEFINITION_SHAPE ( 'NONE', 'NONE',  #15231 ) ;
#15003 = DIRECTION ( 'NONE',  ( 0.000000000000000000, 0.000000000000000000, 1.000000000000000000 ) ) ;
#15004 = EDGE_LOOP ( 'NONE', ( #13855, #774, #11616, #6447, #7070 ) ) ;
#15005 = VERTEX_POINT ( 'NONE', #12508 ) ;
#15006 = ORIENTED_EDGE ( 'NONE', *, *, #3350, .F. ) ;
#15007 = ORIENTED_EDGE ( 'NONE', *, *, #8821, .T. ) ;
#15008 = CARTESIAN_POINT ( 'NONE',  ( -4.747884751462026820, -5.143694235355983579, -0.8000000000000000444 ) ) ;
#15009 = FILL_AREA_STYLE ('',( #4405 ) ) ;
#15010 = EDGE_CURVE ( 'NONE', #6338, #1813, #1982, .T. ) ;
#15011 = DIRECTION ( 'NONE',  ( -1.000000000000000000, 0.000000000000000000, 0.000000000000000000 ) ) ;
#15012 = CARTESIAN_POINT ( 'NONE',  ( 91.12964445316929130, 15.08873975234342701, 3.000000000000000000 ) ) ;
#15013 = VERTEX_POINT ( 'NONE', #6812 ) ;
#15014 = CARTESIAN_POINT ( 'NONE',  ( 2.790000000000011138, -13.12804621868818167, -5.226330906376194463 ) ) ;
#15015 = CARTESIAN_POINT ( 'NONE',  ( 0.5321745227542316048, 19.66801664102731095, -18.57583492944399950 ) ) ;
#15016 = EDGE_CURVE ( 'NONE', #11000, #2791, #10965, .T. ) ;
#15017 = EDGE_CURVE ( 'NONE', #8579, #5309, #11273, .T. ) ;
#15018 = LINE ( 'NONE', #8784, #6934 ) ;
#15019 = VERTEX_POINT ( 'NONE', #6666 ) ;
#15020 = DIRECTION ( 'NONE',  ( 0.000000000000000000, 1.000000000000000000, 1.099230717450651647E-14 ) ) ;
#15021 = FACE_OUTER_BOUND ( 'NONE', #6672, .T. ) ;
#15022 = ORIENTED_EDGE ( 'NONE', *, *, #8016, .F. ) ;
#15023 = ORIENTED_EDGE ( 'NONE', *, *, #9161, .F. ) ;
#15024 = DIRECTION ( 'NONE',  ( -1.000000000000000000, -0.000000000000000000, 0.000000000000000000 ) ) ;
#15025 = EDGE_CURVE ( 'NONE', #9696, #11269, #2046, .T. ) ;
#15026 = ADVANCED_FACE ( 'NONE', ( #10195 ), #1045, .F. ) ;
#15027 = VERTEX_POINT ( 'NONE', #5597 ) ;
#15028 = AXIS2_PLACEMENT_3D ( 'NONE', #1272, #7121, #5965 ) ;
#15029 = LINE ( 'NONE', #2414, #8556 ) ;
#15030 = EDGE_CURVE ( 'NONE', #9599, #6485, #9195, .T. ) ;
#15031 = LINE ( 'NONE', #4661, #11872 ) ;
#15032 = FACE_OUTER_BOUND ( 'NONE', #3537, .T. ) ;
#15033 = VERTEX_POINT ( 'NONE', #8042 ) ;
#15034 = CARTESIAN_POINT ( 'NONE',  ( 2.765633920072237295, 12.59161484032912171, 21.30679549418635688 ) ) ;
#15035 = ORIENTED_EDGE ( 'NONE', *, *, #9017, .T. ) ;
#15036 = VERTEX_POINT ( 'NONE', #12718 ) ;
#15037 = EDGE_CURVE ( 'NONE', #11822, #269, #7101, .T. ) ;
#15038 = TOROIDAL_SURFACE ( 'NONE', #1040, 24.12539914357697413, 8.000000000000000000 ) ;
#15039 = ORIENTED_EDGE ( 'NONE', *, *, #12553, .F. ) ;
#15040 = CARTESIAN_POINT ( 'NONE',  ( -4.000000000000000888, 0.000000000000000000, -10.00000000000000000 ) ) ;
#15041 = DIRECTION ( 'NONE',  ( 0.000000000000000000, 0.000000000000000000, 1.000000000000000000 ) ) ;
#15042 = DIRECTION ( 'NONE',  ( -0.000000000000000000, -0.000000000000000000, -1.000000000000000000 ) ) ;
#15043 = CARTESIAN_POINT ( 'NONE',  ( 0.1085714285714285687, -3.798448662927795372, -0.8000000000000000444 ) ) ;
#15044 = ITEM_DEFINED_TRANSFORMATION ( 'NONE', 'NONE', #824,  #1376 ) ;
#15045 = DIRECTION ( 'NONE',  ( -5.480158469902919838E-17, -1.051478716308701618E-16, -1.000000000000000000 ) ) ;
#15046 = LINE ( 'NONE', #4514, #11050 ) ;
#15047 = ORIENTED_EDGE ( 'NONE', *, *, #9634, .T. ) ;
#15049 = CIRCLE ( 'NONE', #8397, 4.000000000000003553 ) ;
#15048 = CARTESIAN_POINT ( 'NONE',  ( 2.789999999999999147, -13.40591150984221080, -7.739906618939849103 ) ) ;
#15050 = FACE_OUTER_BOUND ( 'NONE', #3043, .T. ) ;
#15051 = CARTESIAN_POINT ( 'NONE',  ( -9.403944755730119454, -7.794738323547949932, 22.00000000000000000 ) ) ;
#15052 = VERTEX_POINT ( 'NONE', #13574 ) ;
#15053 = DIRECTION ( 'NONE',  ( -1.000000000000000000, -0.000000000000000000, -0.000000000000000000 ) ) ;
#15054 = CARTESIAN_POINT ( 'NONE',  ( -1.249999999999998002, 4.599999999999999645, 0.000000000000000000 ) ) ;
#15055 = ORIENTED_EDGE ( 'NONE', *, *, #3097, .F. ) ;
#15056 = ORIENTED_EDGE ( 'NONE', *, *, #12571, .T. ) ;
#15057 = CARTESIAN_POINT ( 'NONE',  ( 2.604434514863827488, -23.63475234378990208, 10.67816411292155543 ) ) ;
#15058 = FACE_OUTER_BOUND ( 'NONE', #5650, .T. ) ;
#15059 = VERTEX_POINT ( 'NONE', #5518 ) ;
#15060 = CARTESIAN_POINT ( 'NONE',  ( 2.715264205769513772, -15.04916547791956205, 2.569134216958844696 ) ) ;
#15061 = CARTESIAN_POINT ( 'NONE',  ( 60.64109936584995353, 31.48746944824151583, -2.000000000000000000 ) ) ;
#15062 = CARTESIAN_POINT ( 'NONE',  ( 2.789999999999999147, 0.000000000000000000, 0.000000000000000000 ) ) ;
#15063 = CARTESIAN_POINT ( 'NONE',  ( 80.00000000000000000, 0.000000000000000000, 3.000000000000000000 ) ) ;
#15064 = CARTESIAN_POINT ( 'NONE',  ( 1.039999999999995595, 20.02152543075345648, 19.67366047555537278 ) ) ;
#15065 = EDGE_LOOP ( 'NONE', ( #12461, #8791, #14435, #5441 ) ) ;
#15066 = CARTESIAN_POINT ( 'NONE',  ( 14.27437366993929579, -27.03703358530833967, 5.000000000000000000 ) ) ;
#15067 = DIRECTION ( 'NONE',  ( -0.000000000000000000, 1.000000000000000000, 1.224646799147353207E-16 ) ) ;
#15068 = ADVANCED_FACE ( 'NONE', ( #12422 ), #4441, .F. ) ;
#15069 = ORIENTED_EDGE ( 'NONE', *, *, #5514, .T. ) ;
#15070 =( LENGTH_UNIT ( ) NAMED_UNIT ( * ) SI_UNIT ( .MILLI., .METRE. ) );
#15071 = VERTEX_POINT ( 'NONE', #9047 ) ;
#15072 = ORIENTED_EDGE ( 'NONE', *, *, #2577, .F. ) ;
#15073 = VERTEX_POINT ( 'NONE', #9123 ) ;
#15074 = CARTESIAN_POINT ( 'NONE',  ( 0.000000000000000000, 0.000000000000000000, 6.999999999999989342 ) ) ;
#15075 = CARTESIAN_POINT ( 'NONE',  ( 0.000000000000000000, 0.000000000000000000, 0.000000000000000000 ) ) ;
#15076 = AXIS2_PLACEMENT_3D ( 'NONE', #9659, #9742, #13108 ) ;
#15077 = DIRECTION ( 'NONE',  ( -0.000000000000000000, 0.000000000000000000, 1.000000000000000000 ) ) ;
#15078 = CARTESIAN_POINT ( 'NONE',  ( 1.894355403937850069, -24.59653223688283674, 12.96989951879399072 ) ) ;
#15079 = EDGE_CURVE ( 'NONE', #2255, #4549, #14814, .T. ) ;
#15080 = UNCERTAINTY_MEASURE_WITH_UNIT (LENGTH_MEASURE( 1.000000000000000082E-05 ), #11232, 'distance_accuracy_value', 'NONE');
#15082 = AXIS2_PLACEMENT_3D ( 'NONE', #5246, #12300, #13533 ) ;
#15081 = DIRECTION ( 'NONE',  ( -1.000000000000000000, 0.000000000000000000, 0.000000000000000000 ) ) ;
#15083 = EDGE_CURVE ( 'NONE', #4155, #5857, #9277, .T. ) ;
#15084 = VERTEX_POINT ( 'NONE', #13012 ) ;
#15085 = TOROIDAL_SURFACE ( 'NONE', #7469, 24.12539914357697768, 8.000000000000000000 ) ;
#15086 = CARTESIAN_POINT ( 'NONE',  ( 8.000000000000000000, 0.000000000000000000, 0.000000000000000000 ) ) ;
#15087 = CARTESIAN_POINT ( 'NONE',  ( 2.789999999999999147, -13.87420763704362514, 1.948757464274123885 ) ) ;
#15088 = ADVANCED_FACE ( 'NONE', ( #5821 ), #12940, .T. ) ;
#15089 = CARTESIAN_POINT ( 'NONE',  ( 0.09203966225857096450, 15.03709480088647865, -2.583706482361959100 ) ) ;
#15090 = CIRCLE ( 'NONE', #6250, 31.62277660168379256 ) ;
#15091 = ORIENTED_EDGE ( 'NONE', *, *, #10599, .T. ) ;
#15092 = DIRECTION ( 'NONE',  ( -1.000000000000000000, -0.000000000000000000, 0.000000000000000000 ) ) ;
#15093 = CARTESIAN_POINT ( 'NONE',  ( 1.394999999999999574, 4.147968289691286614, 27.76164181293053090 ) ) ;
#15094 = ORIENTED_EDGE ( 'NONE', *, *, #1057, .T. ) ;
#15095 = ORIENTED_EDGE ( 'NONE', *, *, #10893, .F. ) ;
#15096 = EDGE_CURVE ( 'NONE', #5438, #626, #94, .T. ) ;
#15097 = EDGE_CURVE ( 'NONE', #9762, #10385, #7055, .T. ) ;
#15098 = CARTESIAN_POINT ( 'NONE',  ( 2.789999999999999147, 20.70663861606293210, -15.04425356660737556 ) ) ;
#15099 = TOROIDAL_SURFACE ( 'NONE', #91, 5.000000000000000000, 0.5999999999999999778 ) ;
#15100 = AXIS2_PLACEMENT_3D ( 'NONE', #3320, #11608, #4482 ) ;
#15101 = ORIENTED_EDGE ( 'NONE', *, *, #9963, .F. ) ;
#15102=STYLED_ITEM('',(#15265),#8904);
#15103 = LINE ( 'NONE', #12429, #13344 ) ;
#15104 = CARTESIAN_POINT ( 'NONE',  ( 2.789999999999999147, -5.229914364928447412, 13.68080036884346917 ) ) ;
#15105 = FACE_OUTER_BOUND ( 'NONE', #11009, .T. ) ;
#15106 = FACE_OUTER_BOUND ( 'NONE', #10984, .T. ) ;
#15107 = ORIENTED_EDGE ( 'NONE', *, *, #15097, .T. ) ;
#15108 = PLANE ( 'NONE',  #8167 ) ;
#15109 = CARTESIAN_POINT ( 'NONE',  ( 0.5537796532149702466, 3.624349476775427181, -16.55730827443876763 ) ) ;
#15110 = VERTEX_POINT ( 'NONE', #8338 ) ;
#15111 = AXIS2_PLACEMENT_3D ( 'NONE', #8101, #10705, #1180 ) ;
#15112 = EDGE_CURVE ( 'NONE', #7568, #14980, #4518, .T. ) ;
#15113 = AXIS2_PLACEMENT_3D ( 'NONE', #4872, #5874, #12990 ) ;
#15114 = AXIS2_PLACEMENT_3D ( 'NONE', #878, #11624, #2193 ) ;
#15115 = ORIENTED_EDGE ( 'NONE', *, *, #2874, .F. ) ;
#15116 = CARTESIAN_POINT ( 'NONE',  ( 0.02436607992776455150, 21.30679549418631780, 12.59161484032919986 ) ) ;
#15117 = CARTESIAN_POINT ( 'NONE',  ( 0.02531912748464718033, -9.232963481057685939, -11.36963888406697087 ) ) ;
#15118 = EDGE_CURVE ( 'NONE', #6121, #15033, #1415, .T. ) ;
#15119 = EDGE_CURVE ( 'NONE', #1742, #8861, #5111, .T. ) ;
#15120 = CARTESIAN_POINT ( 'NONE',  ( -0.1713913650100259145, 6.827405905246493187E-16, -5.575000000000000178 ) ) ;
#15121 = CYLINDRICAL_SURFACE ( 'NONE', #12870, 13.19999999999999929 ) ;
#15122 = CARTESIAN_POINT ( 'NONE',  ( 1.749999999999998002, -19.67366047555515252, -20.02152543075368030 ) ) ;
#15123 = PRODUCT_DEFINITION_SHAPE ( 'NONE', 'NONE',  #15239 ) ;
#15124 = DIRECTION ( 'NONE',  ( -0.000000000000000000, -0.000000000000000000, -1.000000000000000000 ) ) ;
#15125 = AXIS2_PLACEMENT_3D ( 'NONE', #3099, #10086, #3017 ) ;
#15126 = ORIENTED_EDGE ( 'NONE', *, *, #4556, .T. ) ;
#15127 = DIRECTION ( 'NONE',  ( 0.000000000000000000, 1.000000000000000000, -1.084202172485504187E-16 ) ) ;
#15128 = DIRECTION ( 'NONE',  ( -1.000000000000000000, -0.000000000000000000, -0.000000000000000000 ) ) ;
#15129 = CYLINDRICAL_SURFACE ( 'NONE', #11258, 8.400000000000000355 ) ;
#15130 = CARTESIAN_POINT ( 'NONE',  ( 5.566640002541124371E-16, 15.96500990068152426, -18.34424029220094354 ) ) ;
#15131 = ORIENTED_EDGE ( 'NONE', *, *, #12074, .F. ) ;
#15132 = CARTESIAN_POINT ( 'NONE',  ( 2.783068945535914551, -24.42321038836784197, 2.248820353272884542 ) ) ;
#15133 = CIRCLE ( 'NONE', #7279, 2.999999999999988898 ) ;
#15134 = CARTESIAN_POINT ( 'NONE',  ( 2.764680872513937349, -13.68080036884344963, -5.229914364928496262 ) ) ;
#15135 = ORIENTED_EDGE ( 'NONE', *, *, #1503, .T. ) ;
#15136 = ORIENTED_EDGE ( 'NONE', *, *, #8508, .T. ) ;
#15137 = CARTESIAN_POINT ( 'NONE',  ( 2.764680872513208598, 11.36963888406700285, -9.232963481057645083 ) ) ;
#15138 = CIRCLE ( 'NONE', #10224, 10.00000000000000000 ) ;
#15139 = CARTESIAN_POINT ( 'NONE',  ( 2.604434325169353581, 25.77772010606605946, -2.851997810081738027 ) ) ;
#15140 = ORIENTED_EDGE ( 'NONE', *, *, #9172, .F. ) ;
#15141 = PRESENTATION_LAYER_ASSIGNMENT (  '', '', ( #641 ) ) ;
#15142 = CARTESIAN_POINT ( 'NONE',  ( -1.249999999999997558, 0.000000000000000000, 0.000000000000000000 ) ) ;
#15143 = CARTESIAN_POINT ( 'NONE',  ( -18.40394475573011945, -10.79473832354794460, -5.000000000000000000 ) ) ;
#15144 = FACE_OUTER_BOUND ( 'NONE', #9726, .T. ) ;
#15145 = CARTESIAN_POINT ( 'NONE',  ( 0.000000000000000000, -18.28042085475266632, -15.74360496233403239 ) ) ;
#15146 = CYLINDRICAL_SURFACE ( 'NONE', #11750, 4.872650870659752442 ) ;
#15147 = EDGE_CURVE ( 'NONE', #5795, #2494, #6960, .T. ) ;
#15148 = ORIENTED_EDGE ( 'NONE', *, *, #12374, .F. ) ;
#15149 = CIRCLE ( 'NONE', #4344, 4.000000000000000000 ) ;
#15150 = CARTESIAN_POINT ( 'NONE',  ( -5.209999999999999964, 0.000000000000000000, 0.000000000000000000 ) ) ;
#15151 = VECTOR ( 'NONE', #7796, 1000.000000000000000 ) ;
#15152 = DIRECTION ( 'NONE',  ( -1.000000000000000000, 0.000000000000000000, -0.000000000000000000 ) ) ;
#15153 = ORIENTED_EDGE ( 'NONE', *, *, #4859, .T. ) ;
#15154 = CIRCLE ( 'NONE', #8502, 17.95481323787947403 ) ;
#15155 = AXIS2_PLACEMENT_3D ( 'NONE', #4747, #6045, #2508 ) ;
#15156 = DIRECTION ( 'NONE',  ( 0.000000000000000000, 0.000000000000000000, 1.000000000000000000 ) ) ;
#15157 = ORIENTED_EDGE ( 'NONE', *, *, #4570, .F. ) ;
#15158 = ORIENTED_EDGE ( 'NONE', *, *, #7230, .F. ) ;
#15159 = ORIENTED_EDGE ( 'NONE', *, *, #12135, .T. ) ;
#15160 = CARTESIAN_POINT ( 'NONE',  ( 1.394999999999998685, 4.835383649608714585, -17.29145405592683815 ) ) ;
#15161 = CARTESIAN_POINT ( 'NONE',  ( -1.000000000000000000, -6.008326913195983998, 0.000000000000000000 ) ) ;
#15162 = AXIS2_PLACEMENT_3D ( 'NONE', #7276, #5832, #14037 ) ;
#15163 = CARTESIAN_POINT ( 'NONE',  ( 0.5431870686475157584, -11.42270873787283847, -12.54666350726135704 ) ) ;
#15164 = DIRECTION ( 'NONE',  ( -1.000000000000000000, -0.000000000000000000, -0.000000000000000000 ) ) ;
#15165 = ADVANCED_FACE ( 'NONE', ( #10504 ), #7266, .T. ) ;
#15166 = CIRCLE ( 'NONE', #11952, 3.799999999999999378 ) ;
#15167 = CARTESIAN_POINT ( 'NONE',  ( 1.394999999999999574, -17.39253030560844593, 4.458161950358439540 ) ) ;
#15168 = AXIS2_PLACEMENT_3D ( 'NONE', #11190, #351, #501 ) ;
#15169 = VERTEX_POINT ( 'NONE', #15120 ) ;
#15170 = VECTOR ( 'NONE', #12216, 1000.000000000000000 ) ;
#15171 = DIRECTION ( 'NONE',  ( -1.000000000000000000, -0.000000000000000000, -0.000000000000000000 ) ) ;
#15172 = ADVANCED_BREP_SHAPE_REPRESENTATION ( '', ( #3822, #1376 ), #5367 ) ;
#15173 = CARTESIAN_POINT ( 'NONE',  ( 2.789999999999999147, 20.62201879784912606, 12.52067188844359080 ) ) ;
#15174 = EDGE_CURVE ( 'NONE', #11965, #12266, #5958, .T. ) ;
#15175 = AXIS2_PLACEMENT_3D ( 'NONE', #6663, #4358, #5667 ) ;
#15176 = ORIENTED_EDGE ( 'NONE', *, *, #9410, .F. ) ;
#15177 = PRESENTATION_LAYER_ASSIGNMENT (  '', '', ( #1915 ) ) ;
#15178 = CARTESIAN_POINT ( 'NONE',  ( 56.98919079003883326, 3.953582723775848962, 4.000000000000000000 ) ) ;
#15179 = EDGE_CURVE ( 'NONE', #12653, #3644, #4357, .T. ) ;
#15180 = DIRECTION ( 'NONE',  ( -0.6310987668242443727, -0.7757024858236036824, -5.947623346206206400E-19 ) ) ;
#15181 = AXIS2_PLACEMENT_3D ( 'NONE', #2222, #4382, #8982 ) ;
#15182 = ORIENTED_EDGE ( 'NONE', *, *, #7156, .T. ) ;
#15183 = ORIENTED_EDGE ( 'NONE', *, *, #8488, .T. ) ;
#15184 = TOROIDAL_SURFACE ( 'NONE', #7071, 24.12539914357697768, 8.000000000000000000 ) ;
#15185 = CYLINDRICAL_SURFACE ( 'NONE', #13631, 4.000000000000003553 ) ;
#15186 = ORIENTED_EDGE ( 'NONE', *, *, #12909, .T. ) ;
#15187 = FACE_OUTER_BOUND ( 'NONE', #5990, .T. ) ;
#15188 = AXIS2_PLACEMENT_3D ( 'NONE', #11293, #11434, #911 ) ;
#15189 = DIRECTION ( 'NONE',  ( -1.000000000000000000, 0.000000000000000000, -0.000000000000000000 ) ) ;
#15190 = CARTESIAN_POINT ( 'NONE',  ( 67.45386469005195806, 13.93318132202354676, -2.000000000000000888 ) ) ;
#15191 = DIRECTION ( 'NONE',  ( 0.000000000000000000, 0.000000000000000000, 1.000000000000000000 ) ) ;
#15192 = AXIS2_PLACEMENT_3D ( 'NONE', #8862, #10028, #1881 ) ;
#15193 = ORIENTED_EDGE ( 'NONE', *, *, #15214, .T. ) ;
#15194 = AXIS2_PLACEMENT_3D ( 'NONE', #9809, #6193, #4975 ) ;
#15195 = DIRECTION ( 'NONE',  ( -0.000000000000000000, -0.000000000000000000, -1.000000000000000000 ) ) ;
#15196 = DIRECTION ( 'NONE',  ( -1.000000000000000000, -0.000000000000000000, -0.000000000000000000 ) ) ;
#15197 = ORIENTED_EDGE ( 'NONE', *, *, #3329, .F. ) ;
#15198 = ORIENTED_EDGE ( 'NONE', *, *, #901, .T. ) ;
#15199 = CYLINDRICAL_SURFACE ( 'NONE', #11233, 2.000000000000003109 ) ;
#15200 = CARTESIAN_POINT ( 'NONE',  ( 0.000000000000000000, -24.04302995059965653, -1.991882183130557094 ) ) ;
#15201 = EDGE_CURVE ( 'NONE', #11615, #7072, #25, .T. ) ;
#15202 = DIRECTION ( 'NONE',  ( 0.000000000000000000, 0.000000000000000000, 1.000000000000000000 ) ) ;
#15203 = CARTESIAN_POINT ( 'NONE',  ( 1.749999999999998002, 19.67366047555558950, -20.02152543075324687 ) ) ;
#15204 = AXIS2_PLACEMENT_3D ( 'NONE', #1366, #11811, #6063 ) ;
#15205 = ITEM_DEFINED_TRANSFORMATION ( 'NONE', 'NONE', #13336,  #1376 ) ;
#15206 = VECTOR ( 'NONE', #15189, 1000.000000000000000 ) ;
#15207 = DIRECTION ( 'NONE',  ( 0.000000000000000000, 0.000000000000000000, 1.000000000000000000 ) ) ;
#15208 = CYLINDRICAL_SURFACE ( 'NONE', #7868, 2.524999999999999467 ) ;
#15209 = ORIENTED_EDGE ( 'NONE', *, *, #14930, .T. ) ;
#15210 = DIRECTION ( 'NONE',  ( 0.000000000000000000, 0.000000000000000000, -1.000000000000000000 ) ) ;
#15211 = DIRECTION ( 'NONE',  ( 0.000000000000000000, 0.000000000000000000, -1.000000000000000000 ) ) ;
#15212 = CARTESIAN_POINT ( 'NONE',  ( 80.00000000000000000, 0.000000000000000000, 5.500000000000000000 ) ) ;
#15213 = FACE_OUTER_BOUND ( 'NONE', #13154, .T. ) ;
#15214 = EDGE_CURVE ( 'NONE', #6372, #4926, #7463, .T. ) ;
#15215 = EDGE_CURVE ( 'NONE', #9774, #7336, #13685, .T. ) ;
#15216 = ORIENTED_EDGE ( 'NONE', *, *, #12185, .T. ) ;
#15217 = CIRCLE ( 'NONE', #1946, 2.999999999999975131 ) ;
#15218 = VERTEX_POINT ( 'NONE', #8259 ) ;
#15219 = CARTESIAN_POINT ( 'NONE',  ( 0.1374368770859597522, -4.808326913195983821, 0.000000000000000000 ) ) ;
#15220 = ORIENTED_EDGE ( 'NONE', *, *, #5019, .T. ) ;
#15221 = FACE_OUTER_BOUND ( 'NONE', #1761, .T. ) ;
#15222 = ADVANCED_FACE ( 'NONE', ( #12325 ), #12091, .T. ) ;
#15223 = NEXT_ASSEMBLY_USAGE_OCCURRENCE ( 'NAUO1', ' ', ' ', #1381, #12070, $ ) ;
#15224 = NEXT_ASSEMBLY_USAGE_OCCURRENCE ( 'NAUO2', ' ', ' ', #1381, #12917, $ ) ;
#15225 = NEXT_ASSEMBLY_USAGE_OCCURRENCE ( 'NAUO3', ' ', ' ', #1381, #7771, $ ) ;
#15226 = NEXT_ASSEMBLY_USAGE_OCCURRENCE ( 'NAUO4', ' ', ' ', #1381, #11139, $ ) ;
#15227 = NEXT_ASSEMBLY_USAGE_OCCURRENCE ( 'NAUO5', ' ', ' ', #1381, #13870, $ ) ;
#15228 = NEXT_ASSEMBLY_USAGE_OCCURRENCE ( 'NAUO6', ' ', ' ', #1381, #3450, $ ) ;
#15229 = NEXT_ASSEMBLY_USAGE_OCCURRENCE ( 'NAUO7', ' ', ' ', #1381, #3183, $ ) ;
#15230 = NEXT_ASSEMBLY_USAGE_OCCURRENCE ( 'NAUO8', ' ', ' ', #1381, #7771, $ ) ;
#15231 = NEXT_ASSEMBLY_USAGE_OCCURRENCE ( 'NAUO9', ' ', ' ', #1381, #3183, $ ) ;
#15232 = NEXT_ASSEMBLY_USAGE_OCCURRENCE ( 'NAUO10', ' ', ' ', #1381, #3183, $ ) ;
#15233 = NEXT_ASSEMBLY_USAGE_OCCURRENCE ( 'NAUO11', ' ', ' ', #1381, #3183, $ ) ;
#15234 = NEXT_ASSEMBLY_USAGE_OCCURRENCE ( 'NAUO12', ' ', ' ', #1381, #12277, $ ) ;
#15235 = NEXT_ASSEMBLY_USAGE_OCCURRENCE ( 'NAUO13', ' ', ' ', #1381, #12277, $ ) ;
#15236 = NEXT_ASSEMBLY_USAGE_OCCURRENCE ( 'NAUO14', ' ', ' ', #1381, #12277, $ ) ;
#15237 = NEXT_ASSEMBLY_USAGE_OCCURRENCE ( 'NAUO15', ' ', ' ', #1381, #12277, $ ) ;
#15238 = NEXT_ASSEMBLY_USAGE_OCCURRENCE ( 'NAUO16', ' ', ' ', #1381, #11139, $ ) ;
#15239 = NEXT_ASSEMBLY_USAGE_OCCURRENCE ( 'NAUO17', ' ', ' ', #1381, #11139, $ ) ;
#15240 = NEXT_ASSEMBLY_USAGE_OCCURRENCE ( 'NAUO18', ' ', ' ', #1381, #11139, $ ) ;
#15241 = NEXT_ASSEMBLY_USAGE_OCCURRENCE ( 'NAUO19', ' ', ' ', #1381, #6837, $ ) ;
#15242 = NEXT_ASSEMBLY_USAGE_OCCURRENCE ( 'NAUO20', ' ', ' ', #1381, #3183, $ ) ;
#15243 = NEXT_ASSEMBLY_USAGE_OCCURRENCE ( 'NAUO21', ' ', ' ', #1381, #12277, $ ) ;
#15244 = NEXT_ASSEMBLY_USAGE_OCCURRENCE ( 'NAUO22', ' ', ' ', #1381, #12277, $ ) ;
#15245=COLOUR_RGB('Dark Blue',0.08,0.2,0.34);
#15246=FILL_AREA_STYLE_COLOUR('',#15245);
#15247=FILL_AREA_STYLE('',(#15246));
#15248=SURFACE_STYLE_FILL_AREA(#15247);
#15249=SURFACE_SIDE_STYLE('',(#15248));
#15250=SURFACE_STYLE_USAGE(.BOTH.,#15249);
#15251=PRESENTATION_STYLE_ASSIGNMENT((#15250));
#15252=COLOUR_RGB('Light Blue',0.38,0.62,0.78);
#15253=FILL_AREA_STYLE_COLOUR('',#15252);
#15254=FILL_AREA_STYLE('',(#15253));
#15255=SURFACE_STYLE_FILL_AREA(#15254);
#15256=SURFACE_SIDE_STYLE('',(#15255));
#15257=SURFACE_STYLE_USAGE(.BOTH.,#15256);
#15258=PRESENTATION_STYLE_ASSIGNMENT((#15257));
#15259=COLOUR_RGB('Sky Blue',0.24,0.69,0.87);
#15260=FILL_AREA_STYLE_COLOUR('',#15259);
#15261=FILL_AREA_STYLE('',(#15260));
#15262=SURFACE_STYLE_FILL_AREA(#15261);
#15263=SURFACE_SIDE_STYLE('',(#15262));
#15264=SURFACE_STYLE_USAGE(.BOTH.,#15263);
#15265=PRESENTATION_STYLE_ASSIGNMENT((#15264));
#15266=COLOUR_RGB('Grey',0.48,0.52,0.57);
#15267=FILL_AREA_STYLE_COLOUR('',#15266);
#15268=FILL_AREA_STYLE('',(#15267));
#15269=SURFACE_STYLE_FILL_AREA(#15268);
#15270=SURFACE_SIDE_STYLE('',(#15269));
#15271=SURFACE_STYLE_USAGE(.BOTH.,#15270);
#15272=PRESENTATION_STYLE_ASSIGNMENT((#15271));
#15273=COLOUR_RGB('Black',0.12,0.14,0.17);
#15274=FILL_AREA_STYLE_COLOUR('',#15273);
#15275=FILL_AREA_STYLE('',(#15274));
#15276=SURFACE_STYLE_FILL_AREA(#15275);
#15277=SURFACE_SIDE_STYLE('',(#15276));
#15278=SURFACE_STYLE_USAGE(.BOTH.,#15277);
#15279=PRESENTATION_STYLE_ASSIGNMENT((#15278));
#15280=COLOUR_RGB('Off White',0.89,0.88,0.83);
#15281=FILL_AREA_STYLE_COLOUR('',#15280);
#15282=FILL_AREA_STYLE('',(#15281));
#15283=SURFACE_STYLE_FILL_AREA(#15282);
#15284=SURFACE_SIDE_STYLE('',(#15283));
#15285=SURFACE_STYLE_USAGE(.BOTH.,#15284);
#15286=PRESENTATION_STYLE_ASSIGNMENT((#15285));
ENDSEC;
END-ISO-10303-21;
